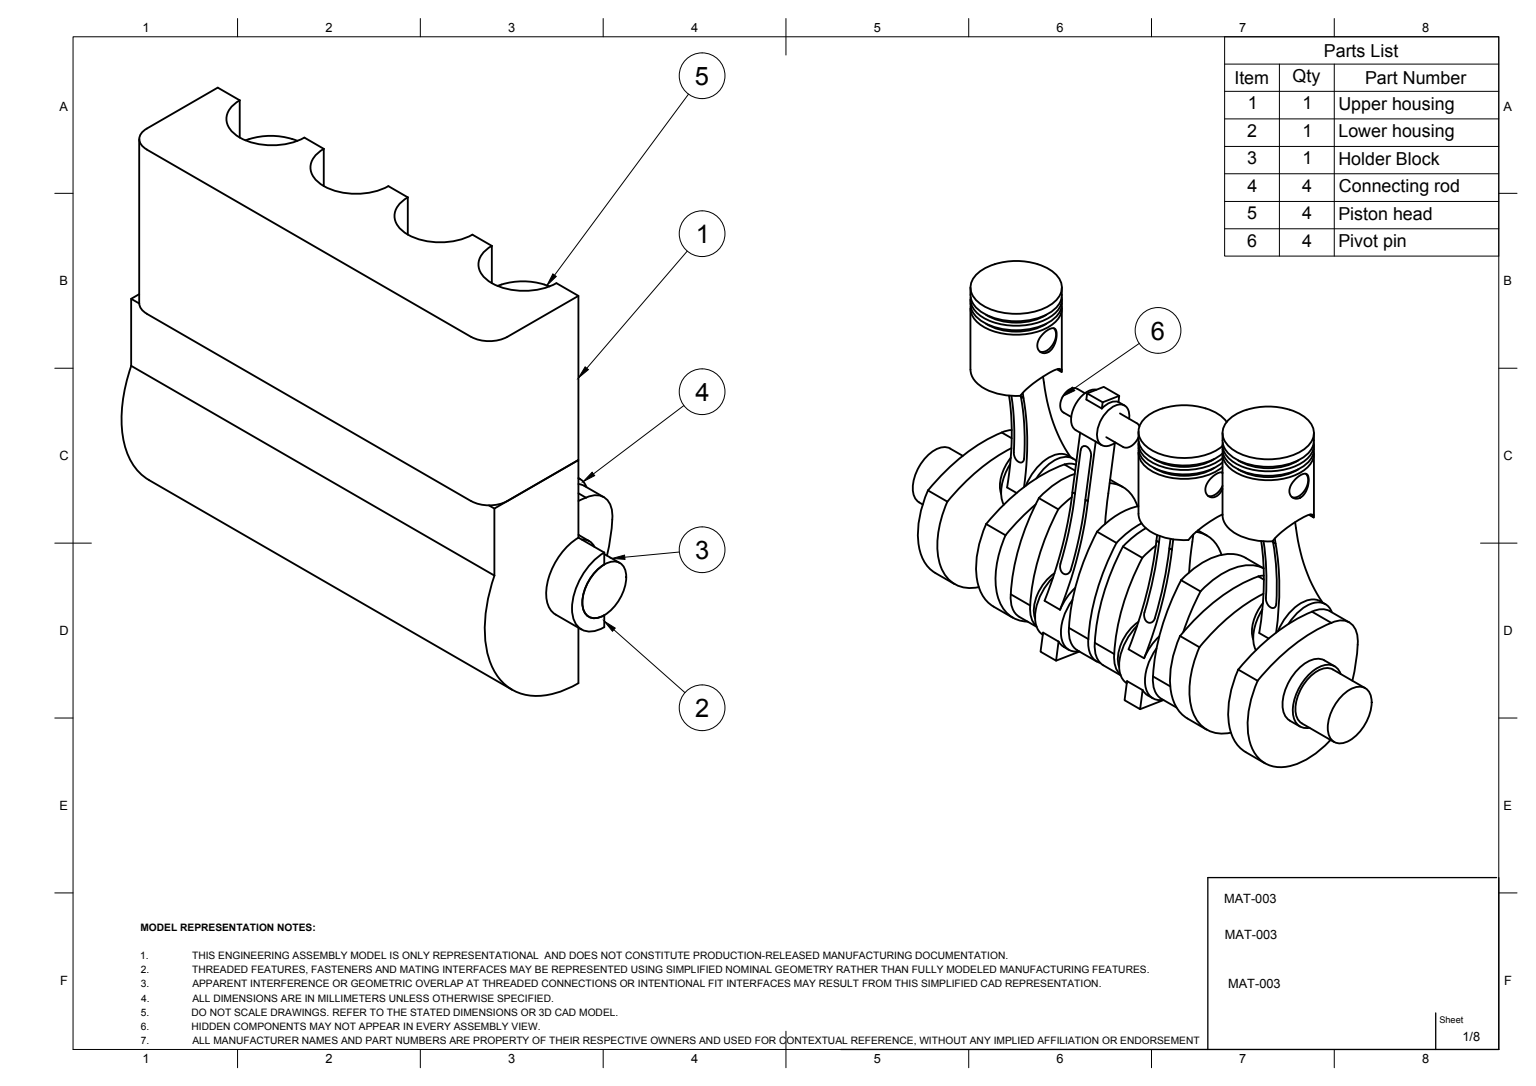
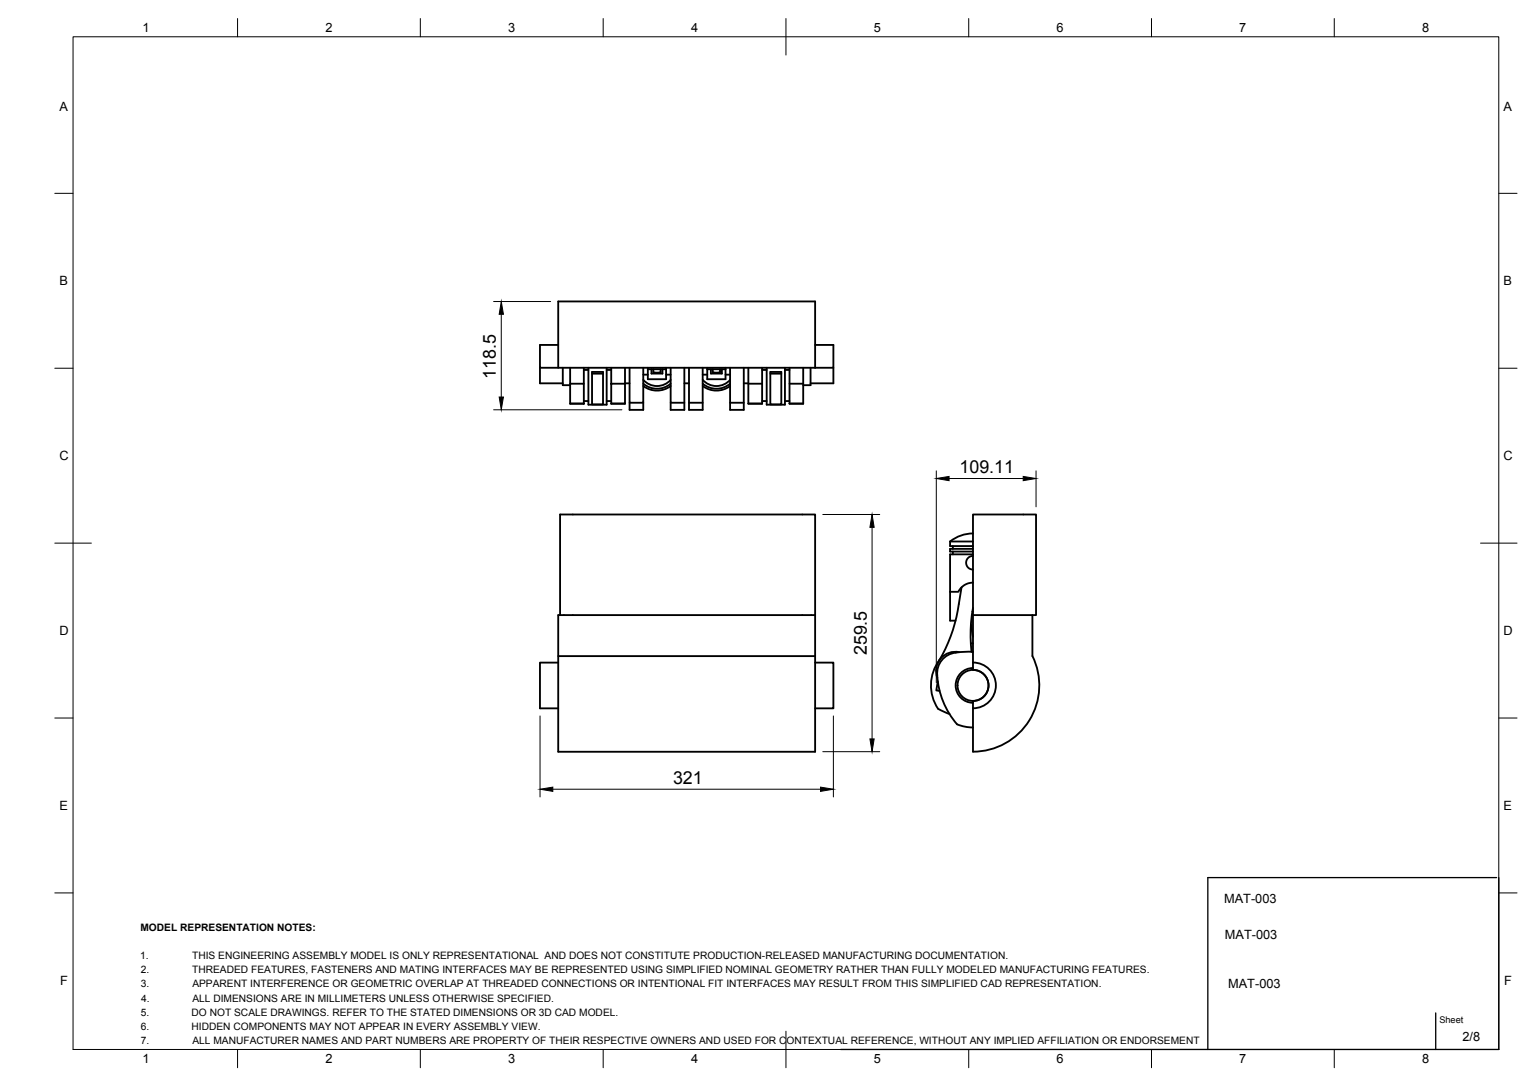
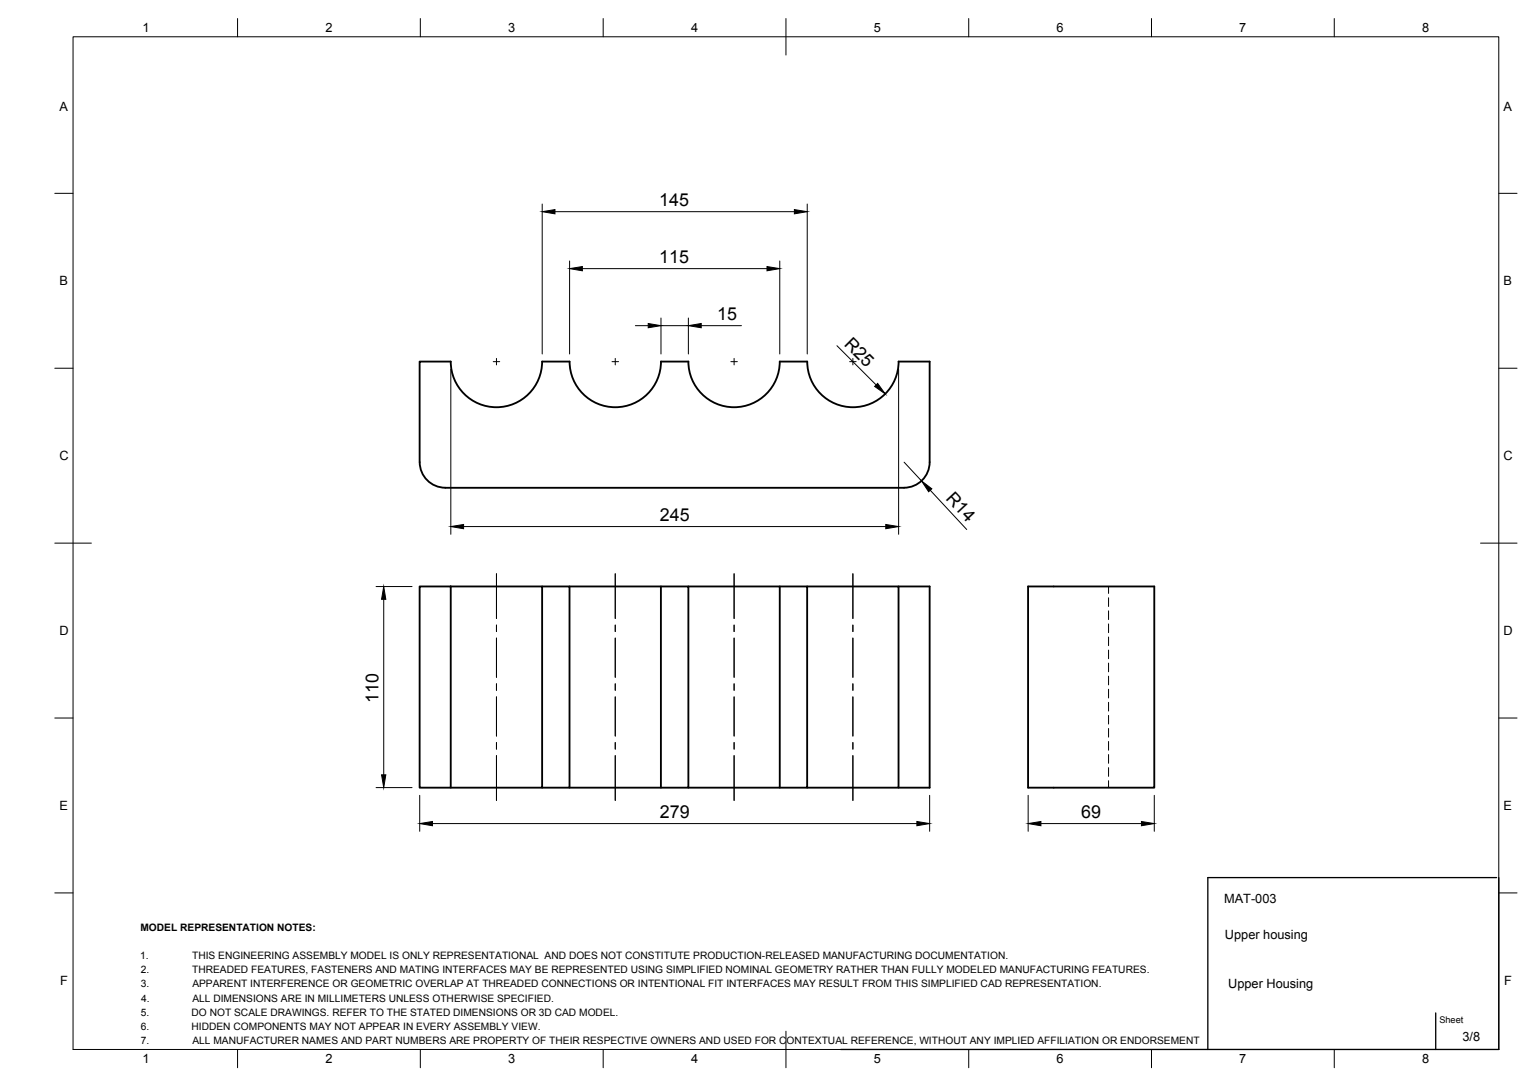
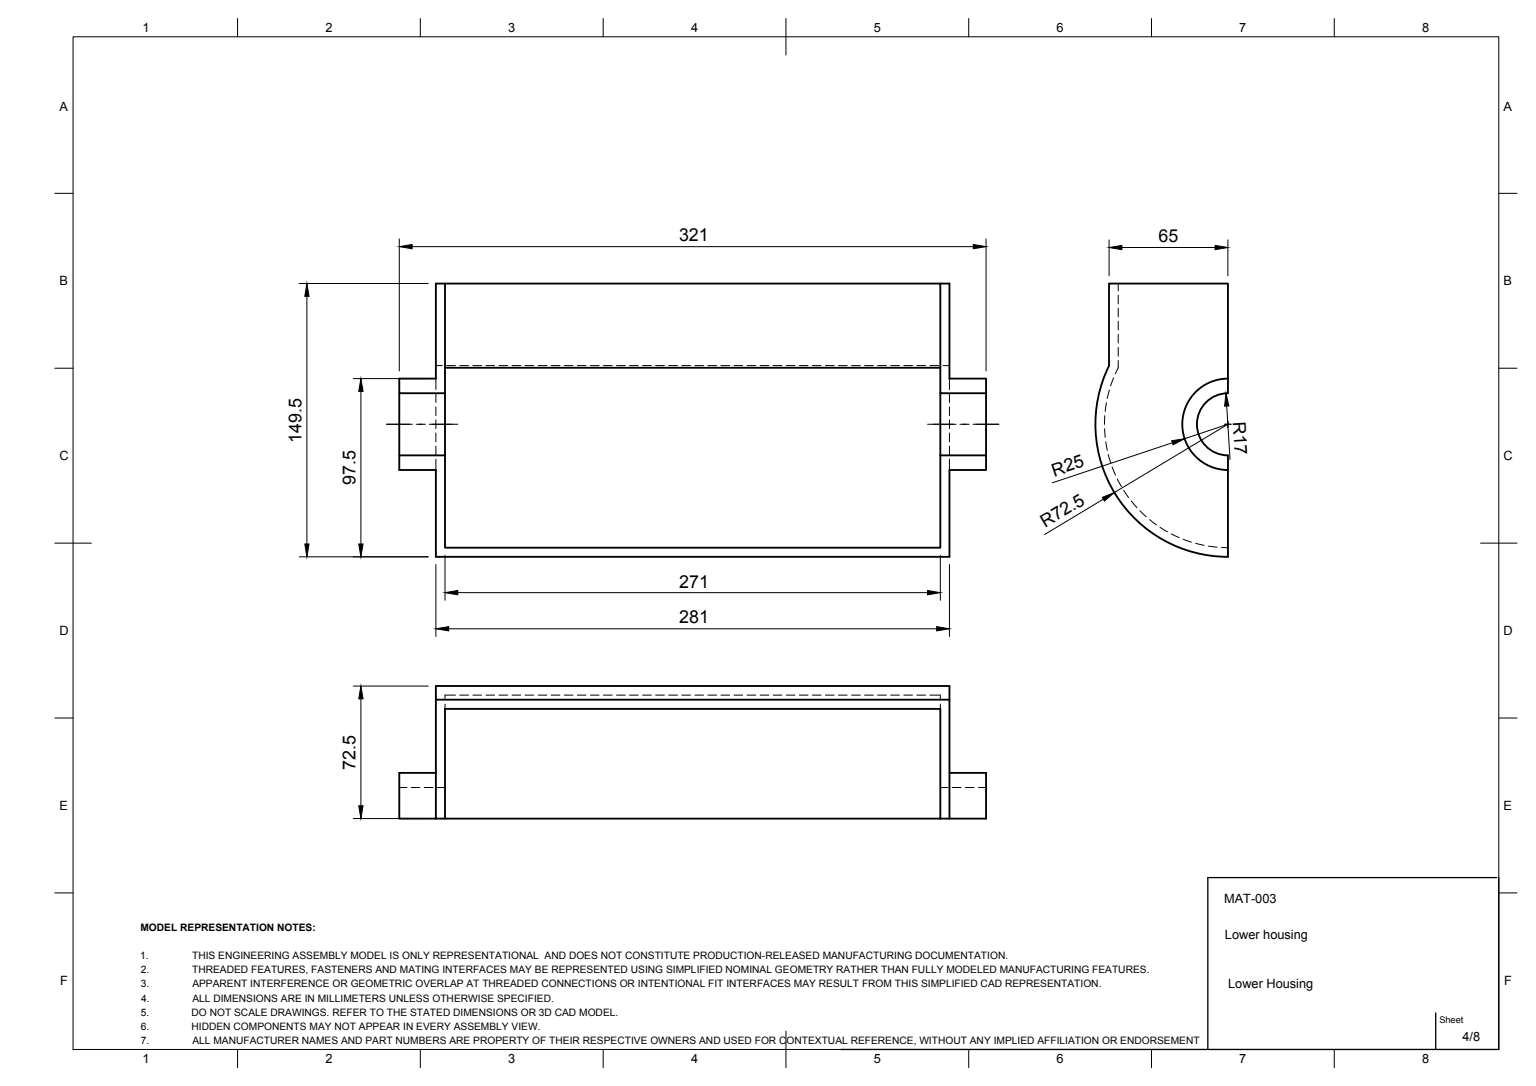
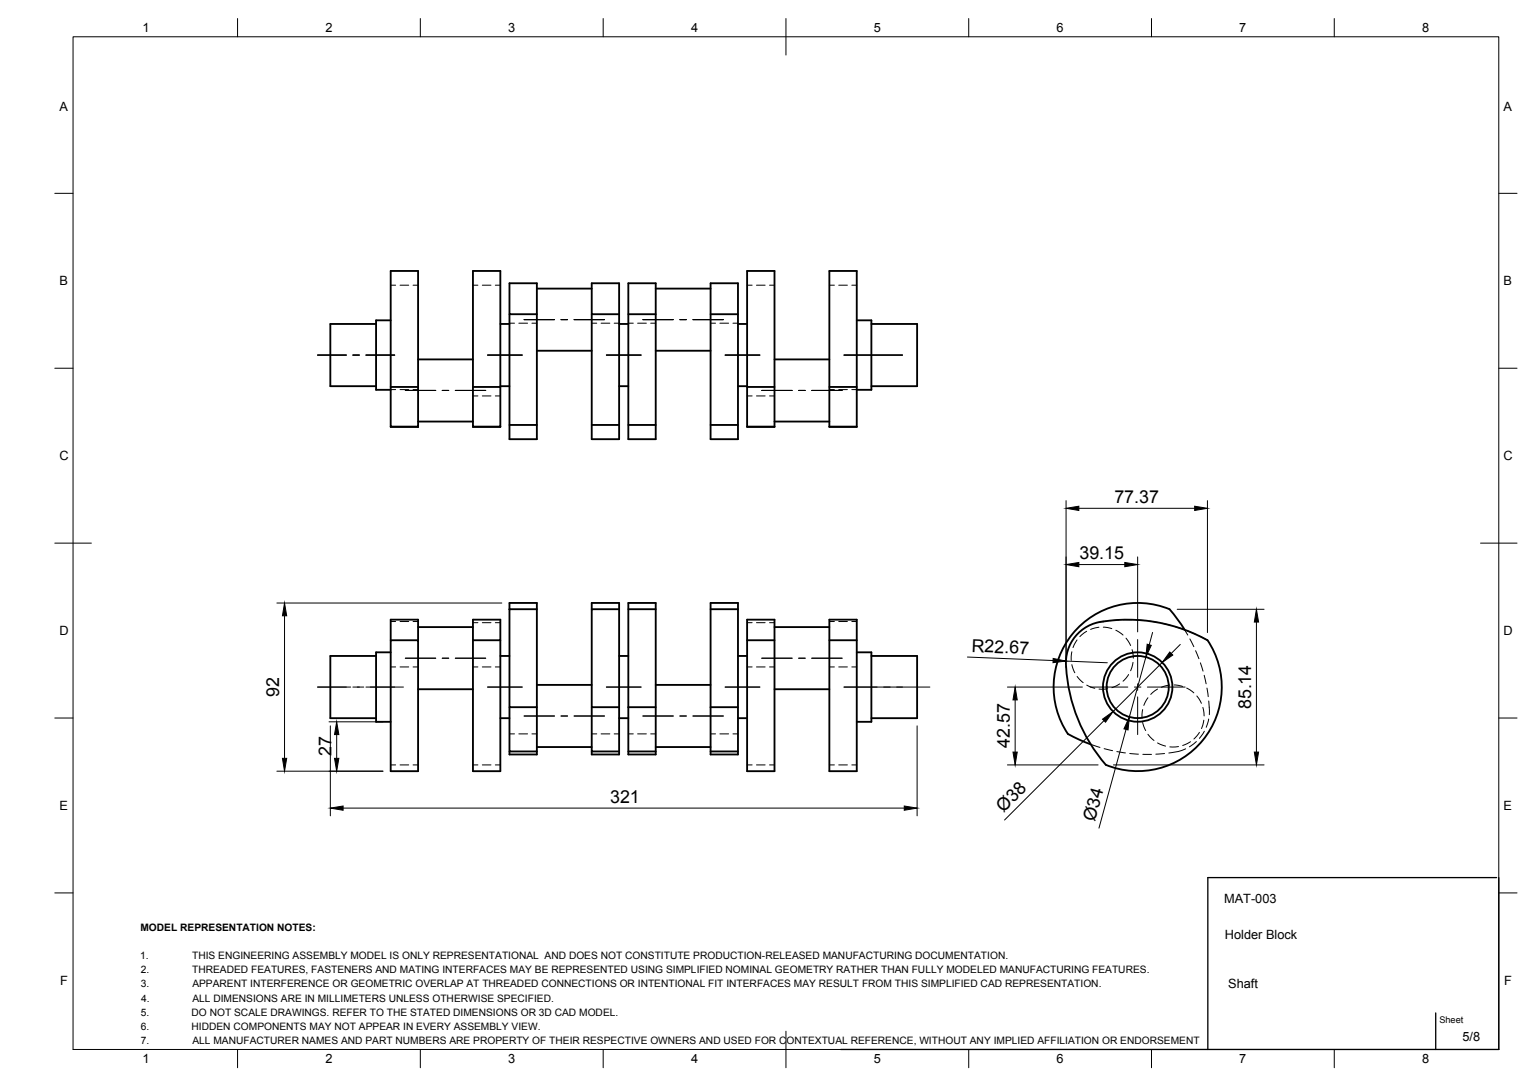
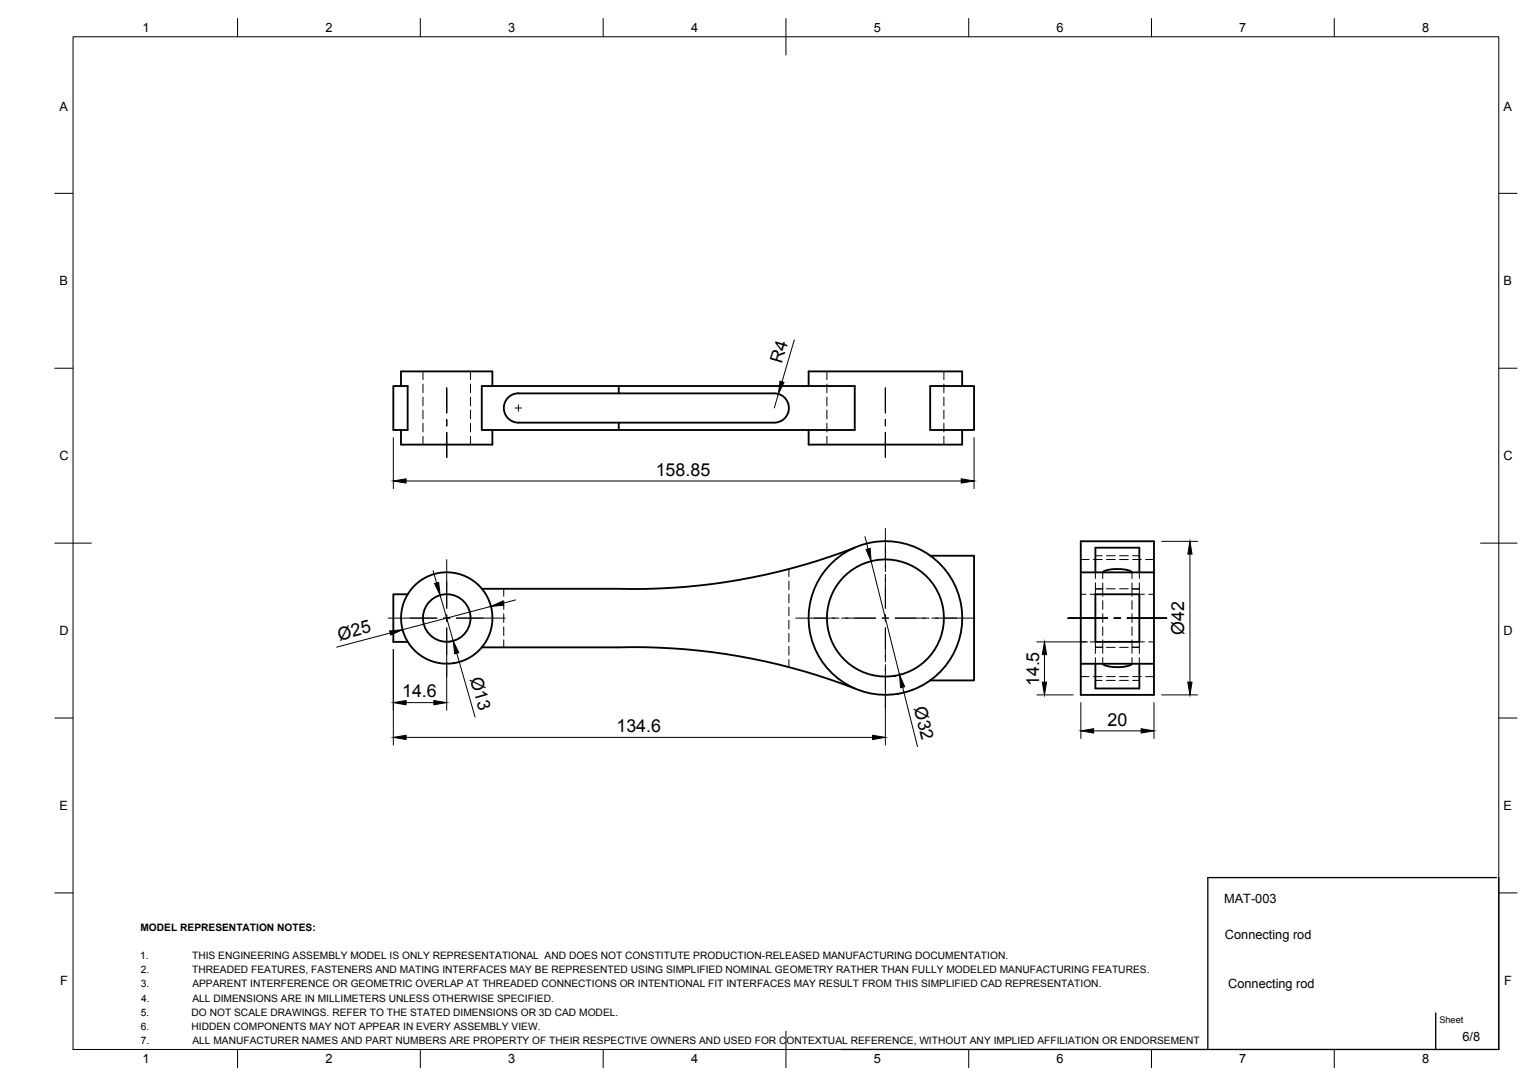
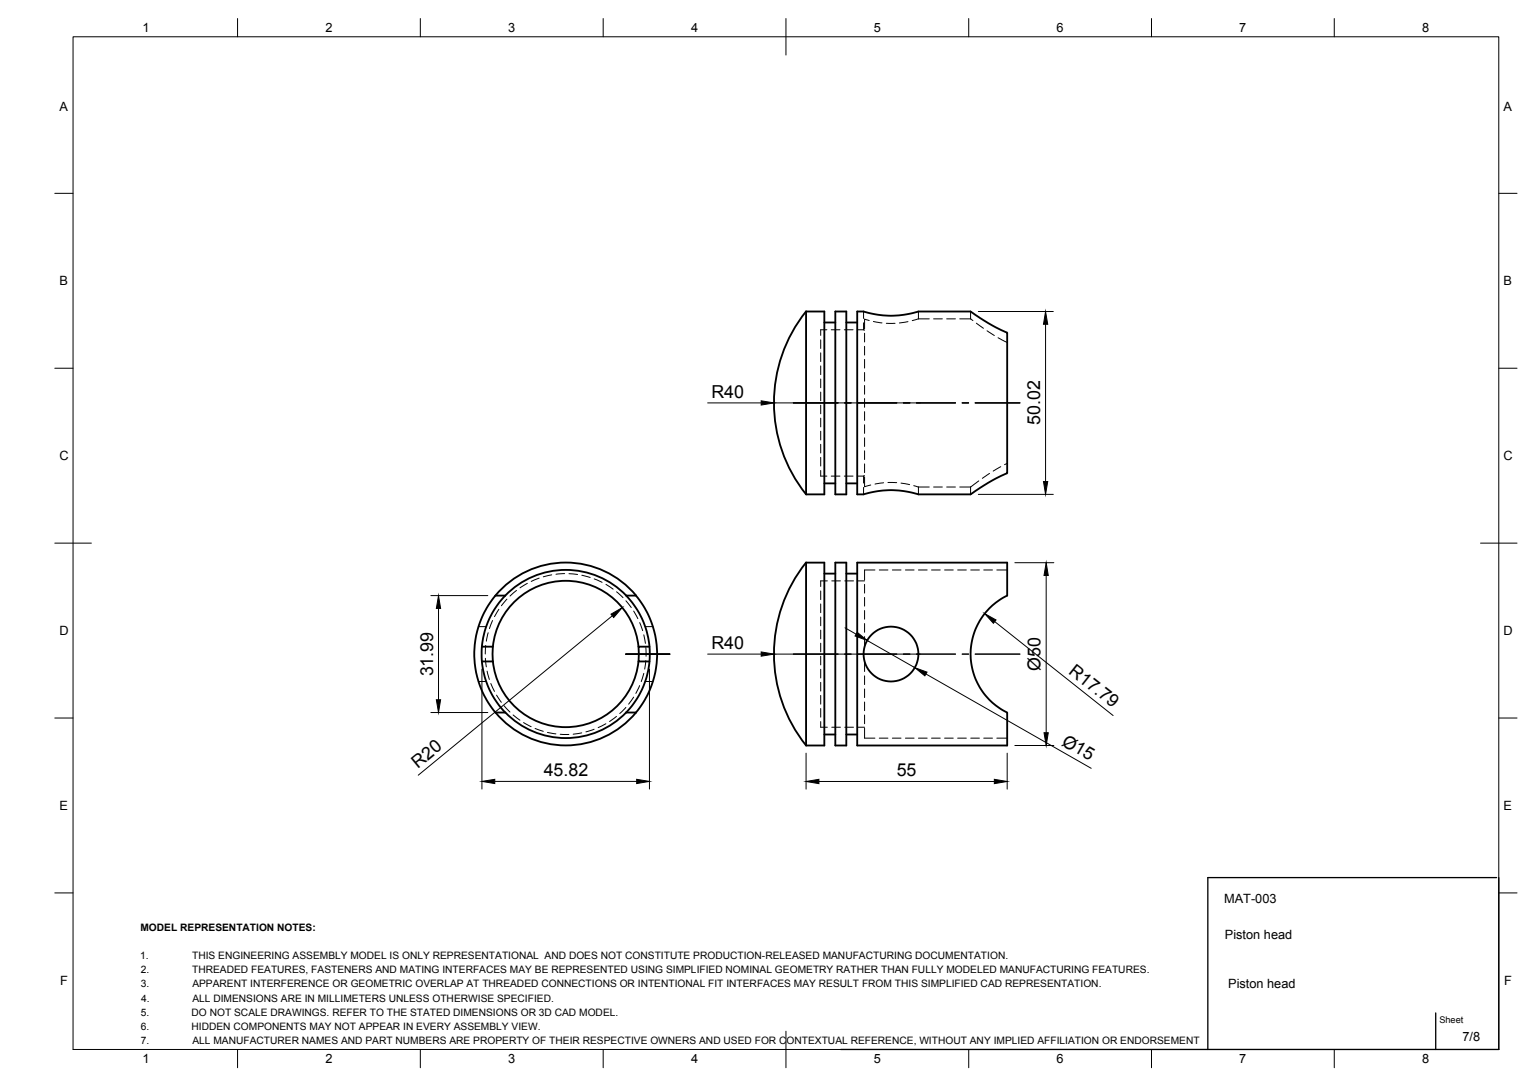
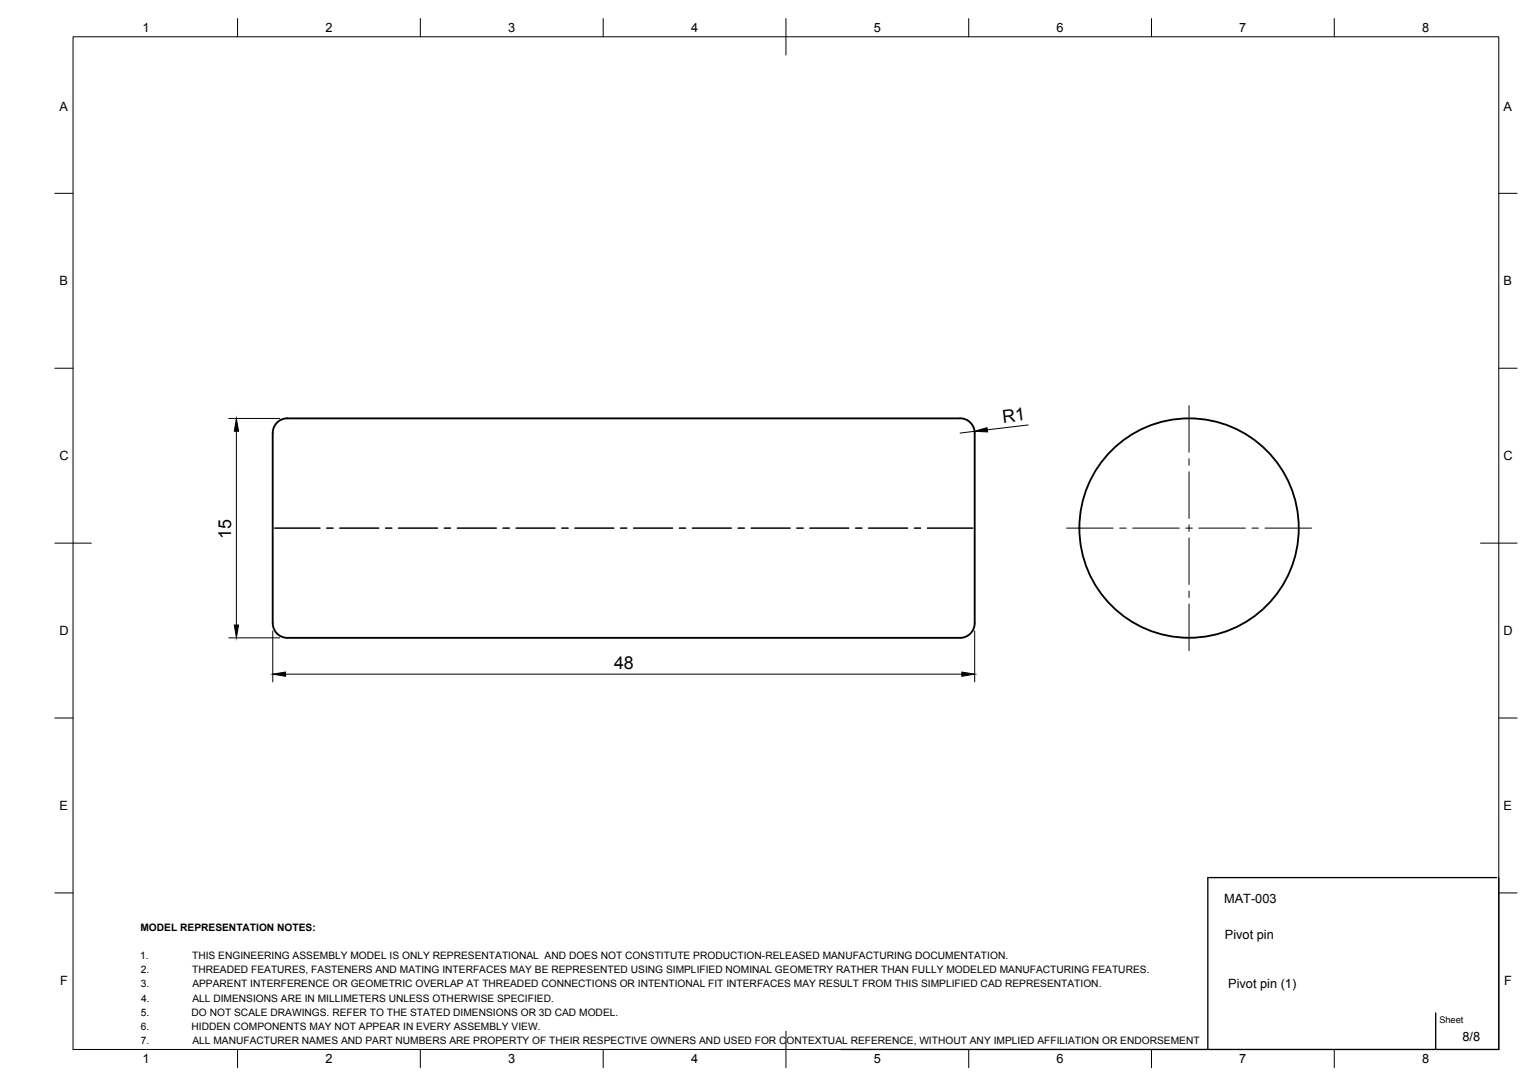
ISO-10303-21;
HEADER;
FILE_DESCRIPTION (('STEP AP214'),
    '1' );
FILE_NAME ('MAT-003',
    '2026-10-10T17:45:43',
    ( '' ),
    ( '' ),
    'SwSTEP 2.0',
    'SolidWorks 2024',
    '' );
FILE_SCHEMA (( 'AUTOMOTIVE_DESIGN' ));
ENDSEC;

DATA;
#1 = DIRECTION ( 'NONE',  ( -1.000000000000000000, 0.000000000000000000, 0.000000000000000000 ) ) ;
#2 = FACE_OUTER_BOUND ( 'NONE', #4262, .T. ) ;
#3 = FACE_OUTER_BOUND ( 'NONE', #4088, .T. ) ;
#4 = VERTEX_POINT ( 'NONE', #461 ) ;
#5 = DIRECTION ( 'NONE',  ( -0.000000000000000000, -0.000000000000000000, -1.000000000000000000 ) ) ;
#6 = AXIS2_PLACEMENT_3D ( 'NONE', #2010, #2938, #1015 ) ;
#7 = PLANE ( 'NONE',  #4575 ) ;
#8 = EDGE_CURVE ( 'NONE', #1209, #6017, #4433, .T. ) ;
#9 = VECTOR ( 'NONE', #5251, 1000.000000000000000 ) ;
#10 = CARTESIAN_POINT ( 'NONE',  ( -13.19762691892552731, 27.23125096863189754, 3.538843351020405148 ) ) ;
#11 = DIRECTION ( 'NONE',  ( -0.000000000000000000, 0.000000000000000000, 1.000000000000000000 ) ) ;
#12 = VERTEX_POINT ( 'NONE', #3966 ) ;
#13 = ORIENTED_EDGE ( 'NONE', *, *, #1970, .T. ) ;
#14 = FACE_OUTER_BOUND ( 'NONE', #2521, .T. ) ;
#15 = AXIS2_PLACEMENT_3D ( 'NONE', #2990, #2506, #3108 ) ;
#16 = FACE_OUTER_BOUND ( 'NONE', #1831, .T. ) ;
#17 = DIRECTION ( 'NONE',  ( -0.000000000000000000, -0.000000000000000000, -1.000000000000000000 ) ) ;
#18 = DIRECTION ( 'NONE',  ( 0.000000000000000000, 1.000000000000000000, 0.000000000000000000 ) ) ;
#19 = EDGE_LOOP ( 'NONE', ( #1698, #4393, #5502, #3759 ) ) ;
#20 = ORIENTED_EDGE ( 'NONE', *, *, #5697, .F. ) ;
#21 = ORIENTED_EDGE ( 'NONE', *, *, #6307, .T. ) ;
#22 = VECTOR ( 'NONE', #3280, 1000.000000000000000 ) ;
#23 = EDGE_CURVE ( 'NONE', #4236, #5003, #2060, .T. ) ;
#24 = DIRECTION ( 'NONE',  ( -0.000000000000000000, -0.000000000000000000, -1.000000000000000000 ) ) ;
#25 = FACE_OUTER_BOUND ( 'NONE', #4505, .T. ) ;
#26 = CARTESIAN_POINT ( 'NONE',  ( 12.21008954351328413, -21.81796696573389127, 5.154724438801038922 ) ) ;
#27 = ORIENTED_EDGE ( 'NONE', *, *, #299, .F. ) ;
#28 = EDGE_CURVE ( 'NONE', #3551, #1184, #4957, .T. ) ;
#29 = EDGE_CURVE ( 'NONE', #4703, #6200, #2516, .T. ) ;
#30 = DIRECTION ( 'NONE',  ( 1.083164259081603456E-16, -1.000000000000000000, 0.000000000000000000 ) ) ;
#31 = CARTESIAN_POINT ( 'NONE',  ( -6.979603745006294879, -21.91560538710199779, 29.02082494059217765 ) ) ;
#32 = EDGE_CURVE ( 'NONE', #4635, #4613, #1964, .T. ) ;
#33 = CARTESIAN_POINT ( 'NONE',  ( 20.00000000000000000, 2.449293598294706513E-15, 39.00000000000001421 ) ) ;
#34 = EDGE_LOOP ( 'NONE', ( #4986, #287, #6272, #1228, #2299, #5503, #2724 ) ) ;
#35 = CARTESIAN_POINT ( 'NONE',  ( 0.000000000000000000, 25.00000000000000000, -30.00000000000000000 ) ) ;
#36 = CIRCLE ( 'NONE', #3210, 17.00000000000000000 ) ;
#37 = CARTESIAN_POINT ( 'NONE',  ( 172.0000000000000000, 68.99999999999998579, 0.000000000000000000 ) ) ;
#38 = B_SPLINE_CURVE_WITH_KNOTS ( 'NONE', 3,
 ( #1697, #6029, #719, #3151, #3705, #4112 ),
 .UNSPECIFIED., .F., .F.,
 ( 4, 2, 4 ),
 ( 0.002032958594636734458, 0.003043324567219494060, 0.004053690539802253662 ),
 .UNSPECIFIED. ) ;
#39 = B_SPLINE_CURVE_WITH_KNOTS ( 'NONE', 3,
 ( #3746, #4279, #1287, #1358, #4178, #783, #2350, #6257, #5782, #1842, #3804, #4739, #3314, #2826, #6155, #5224, #4801, #3253, #3221, #2727, #816, #3709, #5194, #4704, #300, #337, #4247, #6228, #4964, #531, #2445, #3864, #5907, #2482, #4446, #3838, #2858, #3480, #4377, #429, #1973, #1033 ),
 .UNSPECIFIED., .F., .F.,
 ( 4, 2, 2, 2, 2, 2, 2, 2, 2, 2, 2, 2, 2, 2, 2, 2, 2, 2, 2, 2, 4 ),
 ( 0.02358501416070326803, 0.02505868070871360154, 0.02653234725672393851, 0.02800601380473427202, 0.02947968035274460899, 0.03021651362674978442, 0.03095334690075495637, 0.03242701344876530722, 0.03390067999677565114, 0.03463751327078083003, 0.03537434654478600199, 0.03684801309279635284, 0.03758484636680152480, 0.03832167964080669675, 0.03979534618881705454, 0.04126901273682739846, 0.04200584601083257735, 0.04274267928483775625, 0.04421634583284810710, 0.04569001238085845795, 0.04716367892886881574 ),
 .UNSPECIFIED. ) ;
#40 = EDGE_CURVE ( 'NONE', #2876, #1030, #4508, .T. ) ;
#41 = CARTESIAN_POINT ( 'NONE',  ( -16.23652742703189489, -37.28747423195188304, -115.0000000000000000 ) ) ;
#42 = LINE ( 'NONE', #1036, #6075 ) ;
#43 = VERTEX_POINT ( 'NONE', #1427 ) ;
#44 = CARTESIAN_POINT ( 'NONE',  ( 15.23842499831731523, 17.23716120365648052, 1.424676953056493112 ) ) ;
#45 = ORIENTED_EDGE ( 'NONE', *, *, #5504, .T. ) ;
#46 = CARTESIAN_POINT ( 'NONE',  ( -174.7835321302054865, 68.75545066608756883, 12.00000000000000000 ) ) ;
#47 = EDGE_CURVE ( 'NONE', #5003, #1574, #1946, .T. ) ;
#48 = CARTESIAN_POINT ( 'NONE',  ( 73.99999999999987210, 76.99999716619419132, 276.0000000000000000 ) ) ;
#49 = CARTESIAN_POINT ( 'NONE',  ( 17.00000000000000000, 25.00000000000000000, 0.000000000000000000 ) ) ;
#50 = CARTESIAN_POINT ( 'NONE',  ( 64.99991398172927859, 76.99999716619419132, 1.734723475976807094E-15 ) ) ;
#51 = VERTEX_POINT ( 'NONE', #3905 ) ;
#52 = EDGE_LOOP ( 'NONE', ( #3560, #240, #914, #1362 ) ) ;
#53 = VERTEX_POINT ( 'NONE', #142 ) ;
#54 = CARTESIAN_POINT ( 'NONE',  ( 15.99408614349810698, 25.00000000000000000, 0.000000000000000000 ) ) ;
#55 = CARTESIAN_POINT ( 'NONE',  ( -3.061616997868383043E-15, -25.00000000000000000, -65.00000000000000000 ) ) ;
#56 = CARTESIAN_POINT ( 'NONE',  ( -10.32035317195590984, -22.78260342671239869, 6.723738260341698414 ) ) ;
#57 = ORIENTED_EDGE ( 'NONE', *, *, #61, .F. ) ;
#58 = CARTESIAN_POINT ( 'NONE',  ( 31.31180517104795058, 82.87638965790611678, 249.6200851762758077 ) ) ;
#59 = CARTESIAN_POINT ( 'NONE',  ( -7.460990961498263019, -21.75625611239105694, 30.97809455494030928 ) ) ;
#60 = AXIS2_PLACEMENT_3D ( 'NONE', #399, #4931, #2444 ) ;
#61 = EDGE_CURVE ( 'NONE', #5090, #3913, #5607, .T. ) ;
#62 = LINE ( 'NONE', #3376, #3089 ) ;
#63 = ORIENTED_EDGE ( 'NONE', *, *, #4361, .F. ) ;
#64 = B_SPLINE_CURVE_WITH_KNOTS ( 'NONE', 3,
 ( #996, #2949, #3883, #2468, #3228, #4436, #1895, #26, #1990, #4334, #964, #3954, #5828, #5441, #1405, #4365, #5381, #2913, #1023, #549, #5470, #2986, #4820, #446, #5345, #3979, #3401, #2885, #1536, #6336, #4954, #5863, #2503, #4462, #1441, #56, #4887, #4402, #1076, #3622, #4555, #3530, #1685, #4981, #1140, #4096 ),
 .UNSPECIFIED., .F., .F.,
 ( 4, 2, 2, 2, 2, 2, 2, 2, 2, 2, 2, 2, 2, 2, 2, 2, 2, 2, 2, 2, 2, 2, 4 ),
 ( 9.772241184477329324E-19, 0.002589099528182565047, 0.005178199056365129227, 0.006472748820456409799, 0.007767298584547690371, 0.01035639811273024805, 0.01294549764091280919, 0.01424004740500408803, 0.01553459716909536686, 0.01812369669727792107, 0.01941824646136919991, 0.02071279622546047527, 0.02330189575364303295, 0.02459644551773431179, 0.02589099528182559062, 0.02848009481000814483, 0.02977464457409942367, 0.03106919433819069556, 0.03365829386637325671, 0.03495284363046453902, 0.03624739339455581438, 0.03883649292273837206, 0.04142559245092092279 ),
 .UNSPECIFIED. ) ;
#65 = DIRECTION ( 'NONE',  ( 1.000000000000000000, 0.000000000000000000, 0.000000000000000000 ) ) ;
#66 = CIRCLE ( 'NONE', #4486, 12.50000000000001421 ) ;
#67 = LINE ( 'NONE', #4867, #280 ) ;
#68 = COLOUR_RGB ( '',0.7921568627450980005, 0.8196078431372548767, 0.9333333333333333481 ) ;
#69 = EDGE_CURVE ( 'NONE', #1244, #5377, #5049, .T. ) ;
#70 = DIRECTION ( 'NONE',  ( 1.000000000000000000, 0.000000000000000000, 0.000000000000000000 ) ) ;
#71 = ORIENTED_EDGE ( 'NONE', *, *, #5909, .F. ) ;
#72 = VECTOR ( 'NONE', #6322, 1000.000000000000000 ) ;
#73 = FACE_OUTER_BOUND ( 'NONE', #4700, .T. ) ;
#74 = ORIENTED_EDGE ( 'NONE', *, *, #5032, .F. ) ;
#75 = CARTESIAN_POINT ( 'NONE',  ( -0.4497709217647500868, 23.00000000000000355, 24.27501000028010836 ) ) ;
#76 = ADVANCED_FACE ( 'NONE', ( #261, #2578 ), #1123, .T. ) ;
#77 = EDGE_CURVE ( 'NONE', #5794, #1266, #2476, .T. ) ;
#78 = DIRECTION ( 'NONE',  ( -0.000000000000000000, -0.000000000000000000, -1.000000000000000000 ) ) ;
#79 = CARTESIAN_POINT ( 'NONE',  ( 0.000000000000000000, 0.000000000000000000, -240.0000000000000000 ) ) ;
#80 = ORIENTED_EDGE ( 'NONE', *, *, #5837, .T. ) ;
#81 = VERTEX_POINT ( 'NONE', #1223 ) ;
#82 = ORIENTED_EDGE ( 'NONE', *, *, #1705, .T. ) ;
#83 = AXIS2_PLACEMENT_3D ( 'NONE', #303, #4222, #3223 ) ;
#84 = DIRECTION ( 'NONE',  ( 0.000000000000000000, -1.000000000000000000, 0.000000000000000000 ) ) ;
#85 = CARTESIAN_POINT ( 'NONE',  ( 0.000000000000000000, 14.00000000000000000, 0.000000000000000000 ) ) ;
#86 = AXIS2_PLACEMENT_3D ( 'NONE', #5507, #2633, #4633 ) ;
#87 = CARTESIAN_POINT ( 'NONE',  ( 0.000000000000000000, 0.000000000000000000, 48.00000000000000000 ) ) ;
#88 = ORIENTED_EDGE ( 'NONE', *, *, #6209, .F. ) ;
#89 = VECTOR ( 'NONE', #705, 1000.000000000000000 ) ;
#90 = CARTESIAN_POINT ( 'NONE',  ( 0.000000000000000000, -25.00000000000000000, 301.0000000000000568 ) ) ;
#91 = APPLICATION_PROTOCOL_DEFINITION ( 'draft international standard', 'automotive_design', 1998, #867 ) ;
#92 = CARTESIAN_POINT ( 'NONE',  ( -1.353316873173488588, -19.96515186930334096, 39.18355504947043499 ) ) ;
#93 = AXIS2_PLACEMENT_3D ( 'NONE', #1355, #6255, #2382 ) ;
#94 = DIRECTION ( 'NONE',  ( 1.000000000000000000, 0.000000000000000000, 0.000000000000000000 ) ) ;
#95 = EDGE_LOOP ( 'NONE', ( #3114, #6152 ) ) ;
#96 = ORIENTED_EDGE ( 'NONE', *, *, #579, .F. ) ;
#97 = AXIS2_PLACEMENT_3D ( 'NONE', #4292, #3267, #2839 ) ;
#98 = DIRECTION ( 'NONE',  ( -0.000000000000000000, -0.000000000000000000, -1.000000000000000000 ) ) ;
#99 = VECTOR ( 'NONE', #1167, 1000.000000000000000 ) ;
#100 = EDGE_CURVE ( 'NONE', #5003, #2855, #4024, .T. ) ;
#101 = DIRECTION ( 'NONE',  ( 1.000000000000000000, 0.000000000000000000, 0.000000000000000000 ) ) ;
#102 = VECTOR ( 'NONE', #3614, 1000.000000000000000 ) ;
#103 = ADVANCED_BREP_SHAPE_REPRESENTATION ( '', ( #4609, #6349 ), #1927 ) ;
#104 = EDGE_CURVE ( 'NONE', #4120, #4159, #4047, .T. ) ;
#105 = DIRECTION ( 'NONE',  ( 0.000000000000000000, 0.000000000000000000, 1.000000000000000000 ) ) ;
#106 = ORIENTED_EDGE ( 'NONE', *, *, #2540, .F. ) ;
#107 = PRESENTATION_STYLE_ASSIGNMENT (( #4506 ) ) ;
#108 = EDGE_CURVE ( 'NONE', #4284, #2336, #4223, .T. ) ;
#109 = CARTESIAN_POINT ( 'NONE',  ( 279.0000000000000000, 0.000000000000000000, 110.0000000000000000 ) ) ;
#110 = CARTESIAN_POINT ( 'NONE',  ( 0.2247101425308446754, 23.00000000000000355, 24.27501000028010480 ) ) ;
#111 = AXIS2_PLACEMENT_3D ( 'NONE', #2275, #6279, #3332 ) ;
#112 = CARTESIAN_POINT ( 'NONE',  ( 64.99991398172927859, 32.11307465182860454, 281.0000000000000000 ) ) ;
#113 = DIRECTION ( 'NONE',  ( 0.000000000000000000, 0.000000000000000000, -1.000000000000000000 ) ) ;
#114 = ADVANCED_FACE ( 'NONE', ( #2699 ), #6095, .F. ) ;
#115 = VECTOR ( 'NONE', #1796, 1000.000000000000000 ) ;
#116 = VERTEX_POINT ( 'NONE', #626 ) ;
#117 = VERTEX_POINT ( 'NONE', #4668 ) ;
#118 = EDGE_CURVE ( 'NONE', #2855, #4195, #121, .T. ) ;
#119 = EDGE_LOOP ( 'NONE', ( #1237, #139, #1625, #1192 ) ) ;
#120 = CARTESIAN_POINT ( 'NONE',  ( 44.56092774862622719, -29.44644455561813956, -225.0000000000000000 ) ) ;
#121 = CIRCLE ( 'NONE', #637, 24.99999999999999289 ) ;
#122 = AXIS2_PLACEMENT_3D ( 'NONE', #5343, #2370, #5378 ) ;
#123 = CARTESIAN_POINT ( 'NONE',  ( 2.012341796004660122, 22.91179784512888773, 39.00000000000001421 ) ) ;
#124 = CARTESIAN_POINT ( 'NONE',  ( 44.56092774862622719, -29.44644455561813956, -240.0000000000000000 ) ) ;
#125 = EDGE_CURVE ( 'NONE', #1691, #43, #4114, .T. ) ;
#126 = CARTESIAN_POINT ( 'NONE',  ( 0.2052511266213299934, 21.25619793154162807, -45.00000000000000000 ) ) ;
#127 = DIRECTION ( 'NONE',  ( -0.000000000000000000, -0.000000000000000000, 1.000000000000000000 ) ) ;
#128 = ORIENTED_EDGE ( 'NONE', *, *, #3806, .T. ) ;
#129 = AXIS2_PLACEMENT_3D ( 'NONE', #4697, #291, #748 ) ;
#130 = EDGE_CURVE ( 'NONE', #2876, #3788, #5065, .T. ) ;
#131 = DIRECTION ( 'NONE',  ( -0.9999999999999998890, 1.376214178094281264E-17, 4.170629591220277657E-16 ) ) ;
#132 = DIRECTION ( 'NONE',  ( 0.000000000000000000, 1.000000000000000000, 1.247733429937938623E-16 ) ) ;
#133 = CARTESIAN_POINT ( 'NONE',  ( 0.000000000000000000, 0.000000000000000000, 0.000000000000000000 ) ) ;
#134 = ORIENTED_EDGE ( 'NONE', *, *, #595, .T. ) ;
#135 = LINE ( 'NONE', #1113, #2828 ) ;
#136 = UNCERTAINTY_MEASURE_WITH_UNIT (LENGTH_MEASURE( 1.000000000000000082E-05 ), #2437, 'distance_accuracy_value', 'NONE');
#137 = DIRECTION ( 'NONE',  ( -0.000000000000000000, 0.000000000000000000, 1.000000000000000000 ) ) ;
#138 = CYLINDRICAL_SURFACE ( 'NONE', #419, 23.00000000000000000 ) ;
#139 = ORIENTED_EDGE ( 'NONE', *, *, #2354, .F. ) ;
#140 = CARTESIAN_POINT ( 'NONE',  ( 59.99991398172927859, 0.000000000000000000, 281.0000000000000000 ) ) ;
#141 = CIRCLE ( 'NONE', #963, 25.00000000000000000 ) ;
#142 = CARTESIAN_POINT ( 'NONE',  ( -25.00000000000000000, 0.000000000000000000, 0.000000000000000000 ) ) ;
#143 = CARTESIAN_POINT ( 'NONE',  ( -7.491878387983184062, 21.74571065617575982, 31.20484628725278498 ) ) ;
#144 = CARTESIAN_POINT ( 'NONE',  ( 1.698285149303728536, 24.95717370495093945, 9.939986931234113143 ) ) ;
#145 = DIRECTION ( 'NONE',  ( 0.000000000000000000, -1.000000000000000000, 0.000000000000000000 ) ) ;
#146 = VERTEX_POINT ( 'NONE', #1090 ) ;
#147 = ORIENTED_EDGE ( 'NONE', *, *, #6162, .F. ) ;
#148 = ORIENTED_EDGE ( 'NONE', *, *, #974, .F. ) ;
#149 = LINE ( 'NONE', #216, #2805 ) ;
#150 = B_SPLINE_CURVE_WITH_KNOTS ( 'NONE', 3,
 ( #3485, #592, #44, #5457, #3004, #2543, #6001, #2576, #4969, #1575, #4536, #5913, #2094, #979, #2927, #4904, #500, #2450, #1978, #2215, #721, #6123, #4046, #6065, #6032, #5579, #1121, #5643, #2608, #6153, #5126, #1608, #754, #297, #3573, #3219, #1740, #5192, #1644, #234, #5544, #4175 ),
 .UNSPECIFIED., .F., .F.,
 ( 4, 2, 2, 2, 2, 2, 2, 2, 2, 2, 2, 2, 2, 2, 2, 2, 2, 2, 2, 2, 4 ),
 ( 0.000000000000000000, 0.002617858692138167777, 0.005235717384276335554, 0.006544646730345418141, 0.007853576076414500728, 0.01047143476855266243, 0.01308929346069082240, 0.01439822280675990239, 0.01570715215282898758, 0.01832501084496714408, 0.01963394019103622407, 0.02094286953710530058, 0.02356072822924346055, 0.02486965757531254054, 0.02617858692138162399, 0.02879644561351977702, 0.03141430430565794046, 0.03403216299779609350, 0.03665002168993425347, 0.03926788038207241344, 0.04188573907421057341 ),
 .UNSPECIFIED. ) ;
#151 = MANIFOLD_SOLID_BREP ( 'Cut-Extrude1', #5264 ) ;
#152 = CARTESIAN_POINT ( 'NONE',  ( -6.500000000000000000, 134.5953136438507158, 12.00000000000000000 ) ) ;
#153 = DIRECTION ( 'NONE',  ( -0.000000000000000000, -0.000000000000000000, -1.000000000000000000 ) ) ;
#154 = DIRECTION ( 'NONE',  ( -1.000000000000000000, 0.000000000000000000, 0.000000000000000000 ) ) ;
#155 =( GEOMETRIC_REPRESENTATION_CONTEXT ( 3 ) GLOBAL_UNCERTAINTY_ASSIGNED_CONTEXT ( ( #1737 ) ) GLOBAL_UNIT_ASSIGNED_CONTEXT ( ( #6051, #2054, #4037 ) ) REPRESENTATION_CONTEXT ( 'NONE', 'WORKASPACE' ) );
#156 = CYLINDRICAL_SURFACE ( 'NONE', #3481, 4.000000000000000000 ) ;
#157 = VERTEX_POINT ( 'NONE', #5580 ) ;
#158 = FACE_OUTER_BOUND ( 'NONE', #3418, .T. ) ;
#159 = PRODUCT_CONTEXT ( 'NONE', #5893, 'mechanical' ) ;
#160 = LINE ( 'NONE', #6020, #2209 ) ;
#161 = VERTEX_POINT ( 'NONE', #2156 ) ;
#162 = CARTESIAN_POINT ( 'NONE',  ( 0.000000000000000000, 0.000000000000000000, 51.00000000000002842 ) ) ;
#163 = ORIENTED_EDGE ( 'NONE', *, *, #395, .F. ) ;
#164 = DIRECTION ( 'NONE',  ( -0.000000000000000000, -0.000000000000000000, 1.000000000000000000 ) ) ;
#165 = FACE_OUTER_BOUND ( 'NONE', #2771, .T. ) ;
#166 = AXIS2_PLACEMENT_3D ( 'NONE', #680, #1059, #2631 ) ;
#167 = APPLICATION_CONTEXT ( 'automotive_design' ) ;
#168 = DIRECTION ( 'NONE',  ( 1.000000000000000000, 0.000000000000000000, 0.000000000000000000 ) ) ;
#169 = CIRCLE ( 'NONE', #5615, 166.8359700257217071 ) ;
#170 = FACE_OUTER_BOUND ( 'NONE', #5424, .T. ) ;
#171 = ORIENTED_EDGE ( 'NONE', *, *, #4573, .F. ) ;
#172 = CARTESIAN_POINT ( 'NONE',  ( 67.00000000000000000, 69.00000000000000000, 110.0000000000000000 ) ) ;
#173 =( NAMED_UNIT ( * ) PLANE_ANGLE_UNIT ( ) SI_UNIT ( $, .RADIAN. ) );
#174 = CARTESIAN_POINT ( 'NONE',  ( -7.269041597172756219, 21.82161019007790514, 29.87399971471650062 ) ) ;
#175 = AXIS2_PLACEMENT_3D ( 'NONE', #388, #2953, #1897 ) ;
#176 = CARTESIAN_POINT ( 'NONE',  ( -5.944036167333009324, 24.28654258472968763, 8.982995935198127668 ) ) ;
#177 = DIRECTION ( 'NONE',  ( -0.000000000000000000, -0.000000000000000000, -1.000000000000000000 ) ) ;
#178 = EDGE_LOOP ( 'NONE', ( #2214, #4560 ) ) ;
#179 = EDGE_LOOP ( 'NONE', ( #3932, #3010 ) ) ;
#180 = CARTESIAN_POINT ( 'NONE',  ( -17.00000000000000000, 2.081899558550500280E-15, -273.0000000000000000 ) ) ;
#181 = DIRECTION ( 'NONE',  ( -0.000000000000000000, -0.000000000000000000, -1.000000000000000000 ) ) ;
#182 = DIRECTION ( 'NONE',  ( 0.000000000000000000, 1.000000000000000000, -1.284980352575412668E-17 ) ) ;
#183 = DIRECTION ( 'NONE',  ( -0.000000000000000000, -0.000000000000000000, 1.000000000000000000 ) ) ;
#184 = AXIS2_PLACEMENT_3D ( 'NONE', #1992, #4465, #2529 ) ;
#185 = PLANE ( 'NONE',  #3886 ) ;
#186 = ORIENTED_EDGE ( 'NONE', *, *, #4679, .F. ) ;
#187 = EDGE_CURVE ( 'NONE', #1008, #2831, #3637, .T. ) ;
#188 = AXIS2_PLACEMENT_3D ( 'NONE', #6357, #4909, #956 ) ;
#189 = EDGE_CURVE ( 'NONE', #3628, #146, #1775, .T. ) ;
#190 = CARTESIAN_POINT ( 'NONE',  ( -2.450084894395748503, -22.87335089571185875, 38.87807751528530531 ) ) ;
#191 = EDGE_CURVE ( 'NONE', #3657, #5057, #2480, .T. ) ;
#192 = EDGE_LOOP ( 'NONE', ( #4807, #5234, #4644, #6295 ) ) ;
#193 = FACE_OUTER_BOUND ( 'NONE', #676, .T. ) ;
#194 = ORIENTED_EDGE ( 'NONE', *, *, #3413, .T. ) ;
#195 = CIRCLE ( 'NONE', #5537, 17.00000000000000000 ) ;
#196 = EDGE_CURVE ( 'NONE', #1460, #3708, #4019, .T. ) ;
#197 = ADVANCED_FACE ( 'NONE', ( #3287 ), #5676, .F. ) ;
#198 = CARTESIAN_POINT ( 'NONE',  ( 0.000000000000000000, 14.00000000000000000, 110.0000000000000000 ) ) ;
#199 = CARTESIAN_POINT ( 'NONE',  ( -22.21770253897231839, -3.871672004621880436, 0.000000000000000000 ) ) ;
#200 = AXIS2_PLACEMENT_3D ( 'NONE', #653, #2670, #3094 ) ;
#201 = DIRECTION ( 'NONE',  ( 1.000000000000000000, 0.000000000000000000, 0.000000000000000000 ) ) ;
#202 = CARTESIAN_POINT ( 'NONE',  ( 0.000000000000000000, 0.000000000000000000, 0.000000000000000000 ) ) ;
#203 = EDGE_LOOP ( 'NONE', ( #3143, #5565 ) ) ;
#204 = LINE ( 'NONE', #2155, #1735 ) ;
#205 = CIRCLE ( 'NONE', #3492, 45.99999999999997868 ) ;
#206 = DIRECTION ( 'NONE',  ( -0.000000000000000000, -0.000000000000000000, 1.000000000000000000 ) ) ;
#207 = CARTESIAN_POINT ( 'NONE',  ( -3.466163672723409750, 22.74070890941651157, 25.10873389944362444 ) ) ;
#208 = ADVANCED_FACE ( 'NONE', ( #366 ), #2251, .F. ) ;
#209 = CIRCLE ( 'NONE', #6273, 23.00000000000000000 ) ;
#210 = CARTESIAN_POINT ( 'NONE',  ( -13.06023069425439509, 21.31967003585100784, 4.296371343529790110 ) ) ;
#211 = CARTESIAN_POINT ( 'NONE',  ( 3.471216600621237713, -22.73745234227088829, 38.42710443719838054 ) ) ;
#212 = ORIENTED_EDGE ( 'NONE', *, *, #4955, .F. ) ;
#213 = ORIENTED_EDGE ( 'NONE', *, *, #6031, .T. ) ;
#214 = VERTEX_POINT ( 'NONE', #1745 ) ;
#215 = AXIS2_PLACEMENT_3D ( 'NONE', #4568, #5162, #623 ) ;
#216 = CARTESIAN_POINT ( 'NONE',  ( 0.000000000000000000, 76.99999716619419132, 5.000000000000000000 ) ) ;
#217 = CARTESIAN_POINT ( 'NONE',  ( 44.00000000000008527, 13.41640786499836224, -160.0000000000000284 ) ) ;
#218 = DIRECTION ( 'NONE',  ( -0.000000000000000000, -0.000000000000000000, -1.000000000000000000 ) ) ;
#219 = CYLINDRICAL_SURFACE ( 'NONE', #1741, 17.79053956122086078 ) ;
#220 = CARTESIAN_POINT ( 'NONE',  ( 44.43364355155687662, -29.42304313293534790, -45.00000000000000000 ) ) ;
#221 = VERTEX_POINT ( 'NONE', #5746 ) ;
#222 = EDGE_CURVE ( 'NONE', #2940, #959, #39, .T. ) ;
#223 = CARTESIAN_POINT ( 'NONE',  ( -15.63711455316257215, -16.87386736187478675, 0.7328676451471519693 ) ) ;
#224 = ORIENTED_EDGE ( 'NONE', *, *, #2464, .T. ) ;
#225 = DIRECTION ( 'NONE',  ( -0.000000000000000000, 0.000000000000000000, 1.000000000000000000 ) ) ;
#226 = ORIENTED_EDGE ( 'NONE', *, *, #6094, .T. ) ;
#227 = VECTOR ( 'NONE', #4271, 1000.000000000000000 ) ;
#228 = SHAPE_REPRESENTATION_RELATIONSHIP ( 'NONE' , 'NONE' ,  #2313, #2933 ) ;
#229 = CARTESIAN_POINT ( 'NONE',  ( -0.2052511266214760433, -21.25619793154163517, -65.00000000000000000 ) ) ;
#230 = EDGE_CURVE ( 'NONE', #5659, #862, #5842, .T. ) ;
#231 = FACE_OUTER_BOUND ( 'NONE', #5250, .T. ) ;
#232 = CARTESIAN_POINT ( 'NONE',  ( 44.00000000000000000, -13.41640786499873705, -45.00000000000000000 ) ) ;
#233 = ORIENTED_EDGE ( 'NONE', *, *, #2398, .F. ) ;
#234 = CARTESIAN_POINT ( 'NONE',  ( -15.23263781889692048, 17.24245498722747527, 1.434805278142651463 ) ) ;
#235 = DIRECTION ( 'NONE',  ( -0.000000000000000000, -1.740526192617802767E-17, 1.000000000000000000 ) ) ;
#236 = DIRECTION ( 'NONE',  ( -0.000000000000000000, 0.000000000000000000, -1.000000000000000000 ) ) ;
#237 = DIRECTION ( 'NONE',  ( -1.000000000000000000, 0.000000000000000000, 0.000000000000000000 ) ) ;
#238 = DIRECTION ( 'NONE',  ( -1.000000000000000000, 0.000000000000000000, 0.000000000000000000 ) ) ;
#239 = ORIENTED_EDGE ( 'NONE', *, *, #5930, .F. ) ;
#240 = ORIENTED_EDGE ( 'NONE', *, *, #3676, .T. ) ;
#241 = CARTESIAN_POINT ( 'NONE',  ( 0.000000000000000000, 76.99999716619419132, 5.000000000000000000 ) ) ;
#242 = CARTESIAN_POINT ( 'NONE',  ( -0.2052511266214760433, -21.25619793154163517, -160.0000000000000284 ) ) ;
#243 = CARTESIAN_POINT ( 'NONE',  ( 0.000000000000000000, 0.000000000000000000, 55.00000000000000711 ) ) ;
#244 = DIRECTION ( 'NONE',  ( 0.000000000000000000, 0.000000000000000000, -1.000000000000000000 ) ) ;
#245 = FACE_OUTER_BOUND ( 'NONE', #526, .T. ) ;
#246 = EDGE_LOOP ( 'NONE', ( #2762, #958, #1397, #4692, #5981, #2970 ) ) ;
#247 = LINE ( 'NONE', #5691, #4727 ) ;
#248 = DIRECTION ( 'NONE',  ( 1.000000000000000000, 0.000000000000000000, 0.000000000000000000 ) ) ;
#249 = EDGE_CURVE ( 'NONE', #5856, #1997, #4067, .T. ) ;
#250 = ORIENTED_EDGE ( 'NONE', *, *, #4382, .T. ) ;
#251 = PRODUCT_DEFINITION_SHAPE ( 'NONE', 'NONE',  #6365 ) ;
#252 = DIRECTION ( 'NONE',  ( 1.000000000000000000, 0.000000000000000000, 0.000000000000000000 ) ) ;
#253 = ORIENTED_EDGE ( 'NONE', *, *, #3958, .T. ) ;
#254 = DIRECTION ( 'NONE',  ( 1.000000000000000000, 0.000000000000000000, 0.000000000000000000 ) ) ;
#255 = ADVANCED_FACE ( 'NONE', ( #6347, #3897 ), #5362, .T. ) ;
#256 = DIRECTION ( 'NONE',  ( 0.000000000000000000, 0.000000000000000000, 1.000000000000000000 ) ) ;
#257 = CARTESIAN_POINT ( 'NONE',  ( 174.7835321302054865, 68.75545066608756883, 12.00000000000000000 ) ) ;
#258 = VERTEX_POINT ( 'NONE', #1877 ) ;
#259 = DIRECTION ( 'NONE',  ( 0.000000000000000000, 0.000000000000000000, 1.000000000000000000 ) ) ;
#260 = EDGE_LOOP ( 'NONE', ( #5116, #2752, #3718, #1984 ) ) ;
#261 = FACE_OUTER_BOUND ( 'NONE', #2435, .T. ) ;
#262 = CARTESIAN_POINT ( 'NONE',  ( -44.00000000000000000, -13.41640786499873350, -180.0000000000000000 ) ) ;
#263 = AXIS2_PLACEMENT_3D ( 'NONE', #2565, #4526, #132 ) ;
#264 = EDGE_CURVE ( 'NONE', #775, #6000, #3921, .T. ) ;
#265 = CARTESIAN_POINT ( 'NONE',  ( 10.97130857767020551, 22.47473234318869828, 6.237739505811246588 ) ) ;
#267 = ADVANCED_FACE ( 'NONE', ( #945 ), #494, .T. ) ;
#266 = CARTESIAN_POINT ( 'NONE',  ( 5.116921499885075164, -22.42580359959007552, 37.27629952662707069 ) ) ;
#268 = ORIENTED_EDGE ( 'NONE', *, *, #3411, .F. ) ;
#269 = ORIENTED_EDGE ( 'NONE', *, *, #3444, .T. ) ;
#270 = CARTESIAN_POINT ( 'NONE',  ( -0.4986381067920973575, 25.00000000000001066, 24.27501000028010836 ) ) ;
#271 = ADVANCED_FACE ( 'NONE', ( #158 ), #1142, .T. ) ;
#272 = EDGE_CURVE ( 'NONE', #4432, #2238, #5083, .T. ) ;
#273 = LINE ( 'NONE', #4092, #6243 ) ;
#274 = CARTESIAN_POINT ( 'NONE',  ( 0.000000000000000000, 0.000000000000000000, 44.00000000000000711 ) ) ;
#275 = DIRECTION ( 'NONE',  ( -1.000000000000000000, 0.000000000000000000, 0.000000000000000000 ) ) ;
#276 = VECTOR ( 'NONE', #3647, 1000.000000000000000 ) ;
#277 = EDGE_LOOP ( 'NONE', ( #2977, #5435, #3484, #3552 ) ) ;
#278 = CARTESIAN_POINT ( 'NONE',  ( 0.000000000000000000, 0.000000000000000000, -115.0000000000000000 ) ) ;
#279 = ORIENTED_EDGE ( 'NONE', *, *, #1801, .T. ) ;
#280 = VECTOR ( 'NONE', #5453, 1000.000000000000000 ) ;
#281 = CARTESIAN_POINT ( 'NONE',  ( -13.41482486054668044, 26.39531364385071299, 5.999999999999990230 ) ) ;
#282 = APPLICATION_PROTOCOL_DEFINITION ( 'draft international standard', 'automotive_design', 1998, #1178 ) ;
#283 = CARTESIAN_POINT ( 'NONE',  ( 10.37037532854004418, -20.54332595864094202, 6.688011403969689184 ) ) ;
#284 = CIRCLE ( 'NONE', #4395, 22.00000000000000000 ) ;
#285 = ORIENTED_EDGE ( 'NONE', *, *, #6012, .F. ) ;
#286 = CYLINDRICAL_SURFACE ( 'NONE', #1017, 45.99999999999997868 ) ;
#287 = ORIENTED_EDGE ( 'NONE', *, *, #1156, .F. ) ;
#288 = VECTOR ( 'NONE', #565, 1000.000000000000000 ) ;
#289 = DIRECTION ( 'NONE',  ( -1.000000000000000000, 0.000000000000000000, 0.000000000000000000 ) ) ;
#290 = CARTESIAN_POINT ( 'NONE',  ( 0.000000000000000000, 0.000000000000000000, 0.000000000000000000 ) ) ;
#291 = DIRECTION ( 'NONE',  ( -0.000000000000000000, -0.000000000000000000, -1.000000000000000000 ) ) ;
#292 = CARTESIAN_POINT ( 'NONE',  ( 44.00000000000000000, -13.41640786499873705, -45.00000000000000000 ) ) ;
#293 = AXIS2_PLACEMENT_3D ( 'NONE', #3650, #5626, #3015 ) ;
#294 = AXIS2_PLACEMENT_3D ( 'NONE', #2245, #5189, #5257 ) ;
#295 = CARTESIAN_POINT ( 'NONE',  ( -2.426466830553623222, -24.88612820222272148, 38.88851386838337731 ) ) ;
#296 = ORIENTED_EDGE ( 'NONE', *, *, #3074, .T. ) ;
#297 = CARTESIAN_POINT ( 'NONE',  ( -10.37037532854004418, 20.54332595864094202, 6.688011403969689184 ) ) ;
#298 = ORIENTED_EDGE ( 'NONE', *, *, #69, .T. ) ;
#299 = EDGE_CURVE ( 'NONE', #686, #51, #842, .T. ) ;
#300 = CARTESIAN_POINT ( 'NONE',  ( 7.246617758453442804, 23.92680898849839721, 29.82624669321133126 ) ) ;
#301 = CARTESIAN_POINT ( 'NONE',  ( 44.43364355155687662, -29.42304313293534790, -180.0000000000000000 ) ) ;
#302 = AXIS2_PLACEMENT_3D ( 'NONE', #35, #5903, #5416 ) ;
#303 = CARTESIAN_POINT ( 'NONE',  ( 0.000000000000000000, 120.0000000000000000, -4.000000000000000000 ) ) ;
#304 = CARTESIAN_POINT ( 'NONE',  ( 7.306265819825862096, -23.90859775135293219, 30.06340984243352921 ) ) ;
#305 = EDGE_CURVE ( 'NONE', #5346, #4831, #1115, .T. ) ;
#306 = VERTEX_POINT ( 'NONE', #1172 ) ;
#307 = CARTESIAN_POINT ( 'NONE',  ( -3.336113272159680676, 24.78061407909199687, 25.03989924742864304 ) ) ;
#308 = VECTOR ( 'NONE', #2366, 1000.000000000000000 ) ;
#309 = VECTOR ( 'NONE', #6106, 1000.000000000000000 ) ;
#310 = DIRECTION ( 'NONE',  ( 1.000000000000000000, 0.000000000000000000, 0.000000000000000000 ) ) ;
#311 = CIRCLE ( 'NONE', #916, 25.00000000000000000 ) ;
#312 = DIRECTION ( 'NONE',  ( -0.000000000000000000, 0.000000000000000000, -1.000000000000000000 ) ) ;
#313 = EDGE_CURVE ( 'NONE', #2336, #4284, #725, .T. ) ;
#314 = FACE_BOUND ( 'NONE', #5611, .T. ) ;
#315 = EDGE_CURVE ( 'NONE', #1906, #997, #247, .T. ) ;
#316 = AXIS2_PLACEMENT_3D ( 'NONE', #4448, #5394, #4967 ) ;
#317 = ORIENTED_EDGE ( 'NONE', *, *, #272, .T. ) ;
#318 = CARTESIAN_POINT ( 'NONE',  ( -8.000000000000021316, 1.481987083124922376E-15, 12.00000000000000000 ) ) ;
#319 = ORIENTED_EDGE ( 'NONE', *, *, #4152, .T. ) ;
#320 = DIRECTION ( 'NONE',  ( -0.000000000000000000, -0.000000000000000000, 1.000000000000000000 ) ) ;
#321 = AXIS2_PLACEMENT_3D ( 'NONE', #133, #3087, #5016 ) ;
#322 = EDGE_CURVE ( 'NONE', #5682, #117, #4160, .T. ) ;
#323 = CARTESIAN_POINT ( 'NONE',  ( -4.378668635177231927, -22.59503479412315485, 9.474032806803469597 ) ) ;
#324 = ORIENTED_EDGE ( 'NONE', *, *, #5982, .T. ) ;
#325 = CARTESIAN_POINT ( 'NONE',  ( -19.00000000000000000, 2.326828918379970970E-15, -248.0000000000000000 ) ) ;
#326 = ORIENTED_EDGE ( 'NONE', *, *, #3688, .T. ) ;
#327 = EDGE_CURVE ( 'NONE', #4956, #1995, #4828, .T. ) ;
#328 = VECTOR ( 'NONE', #3380, 1000.000000000000000 ) ;
#329 = AXIS2_PLACEMENT_3D ( 'NONE', #4721, #320, #1790 ) ;
#330 = SHAPE_REPRESENTATION_RELATIONSHIP ( 'NONE' , 'NONE' ,  #5199, #2789 ) ;
#331 = DIRECTION ( 'NONE',  ( -0.000000000000000000, -0.000000000000000000, -1.000000000000000000 ) ) ;
#332 = DIRECTION ( 'NONE',  ( 0.000000000000000000, 1.740526192617802767E-17, -1.000000000000000000 ) ) ;
#333 = DIRECTION ( 'NONE',  ( -1.000000000000000000, 0.000000000000000000, 0.000000000000000000 ) ) ;
#334 = ORIENTED_EDGE ( 'NONE', *, *, #1705, .F. ) ;
#335 =( NAMED_UNIT ( * ) PLANE_ANGLE_UNIT ( ) SI_UNIT ( $, .RADIAN. ) );
#336 = VERTEX_POINT ( 'NONE', #3204 ) ;
#337 = CARTESIAN_POINT ( 'NONE',  ( 7.102515314070983798, 23.96997983984566361, 29.35314634237167297 ) ) ;
#338 = CARTESIAN_POINT ( 'NONE',  ( 59.99991398172927859, 8.702630963089024930E-17, 276.0000000000000000 ) ) ;
#339 = CARTESIAN_POINT ( 'NONE',  ( 132.0000000000000000, 69.00000000000000000, 0.000000000000000000 ) ) ;
#340 = CARTESIAN_POINT ( 'NONE',  ( 7.059265739357024394, -21.89000174688035827, 29.23188816227238362 ) ) ;
#341 = VERTEX_POINT ( 'NONE', #281 ) ;
#342 = ORIENTED_EDGE ( 'NONE', *, *, #3066, .F. ) ;
#343 = CARTESIAN_POINT ( 'NONE',  ( -0.4915545007834206670, 24.99637963107063499, 39.26296923598712851 ) ) ;
#344 = DIRECTION ( 'NONE',  ( 1.000000000000000000, 0.000000000000000000, 0.000000000000000000 ) ) ;
#345 = CARTESIAN_POINT ( 'NONE',  ( 265.0000000000000000, 0.000000000000000000, 110.0000000000000000 ) ) ;
#346 = FACE_OUTER_BOUND ( 'NONE', #5806, .T. ) ;
#347 = EDGE_LOOP ( 'NONE', ( #3523, #3999, #1718, #5180 ) ) ;
#348 = ORIENTED_EDGE ( 'NONE', *, *, #5467, .F. ) ;
#349 = ORIENTED_EDGE ( 'NONE', *, *, #5310, .T. ) ;
#350 = AXIS2_PLACEMENT_3D ( 'NONE', #4646, #3102, #2588 ) ;
#351 = CARTESIAN_POINT ( 'NONE',  ( 0.000000000000000000, 0.000000000000000000, 0.000000000000000000 ) ) ;
#352 = CARTESIAN_POINT ( 'NONE',  ( 3.009099790203600300, -22.80648947684007410, 9.749155414846011780 ) ) ;
#353 = DIRECTION ( 'NONE',  ( -1.000000000000000000, 0.000000000000000000, 0.000000000000000000 ) ) ;
#354 = EDGE_LOOP ( 'NONE', ( #837, #2657 ) ) ;
#355 = DIRECTION ( 'NONE',  ( -1.000000000000000000, 0.000000000000000000, 0.000000000000000000 ) ) ;
#356 = ORIENTED_EDGE ( 'NONE', *, *, #2582, .T. ) ;
#357 = FILL_AREA_STYLE_COLOUR ( '', #68 ) ;
#358 = EDGE_CURVE ( 'NONE', #4881, #53, #311, .T. ) ;
#359 = DIRECTION ( 'NONE',  ( 0.000000000000000000, 0.000000000000000000, 1.000000000000000000 ) ) ;
#360 = DIRECTION ( 'NONE',  ( -0.000000000000000000, -0.000000000000000000, -1.000000000000000000 ) ) ;
#361 = CARTESIAN_POINT ( 'NONE',  ( -4.953190041214019068, -24.50516424074860922, 26.13799397941500757 ) ) ;
#362 = ORIENTED_EDGE ( 'NONE', *, *, #5906, .F. ) ;
#363 = EDGE_CURVE ( 'NONE', #4783, #2333, #5736, .T. ) ;
#364 = DIRECTION ( 'NONE',  ( -0.000000000000000000, -0.000000000000000000, -1.000000000000000000 ) ) ;
#365 = MANIFOLD_SOLID_BREP ( 'Cut-Extrude4', #5984 ) ;
#366 = FACE_OUTER_BOUND ( 'NONE', #4514, .T. ) ;
#367 = DIRECTION ( 'NONE',  ( -0.000000000000000000, -0.000000000000000000, -1.000000000000000000 ) ) ;
#368 = DIRECTION ( 'NONE',  ( 0.000000000000000000, 0.000000000000000000, -1.000000000000000000 ) ) ;
#369 = CARTESIAN_POINT ( 'NONE',  ( 7.450717329638294473, -23.86413627455948117, 32.76425935539838008 ) ) ;
#370 = ORIENTED_EDGE ( 'NONE', *, *, #6217, .T. ) ;
#371 = VERTEX_POINT ( 'NONE', #5182 ) ;
#372 = CARTESIAN_POINT ( 'NONE',  ( -7.499773188859400364, 23.84855136421925437, 31.27916535100971274 ) ) ;
#373 = DIRECTION ( 'NONE',  ( 0.000000000000000000, 0.000000000000000000, 1.000000000000000000 ) ) ;
#374 = DIRECTION ( 'NONE',  ( 1.000000000000000000, 0.000000000000000000, 0.000000000000000000 ) ) ;
#375 = AXIS2_PLACEMENT_3D ( 'NONE', #3837, #2921, #5808 ) ;
#376 = CARTESIAN_POINT ( 'NONE',  ( 0.000000000000000000, 0.000000000000000000, 0.000000000000000000 ) ) ;
#377 = AXIS2_PLACEMENT_3D ( 'NONE', #2646, #5558, #3130 ) ;
#378 = ORIENTED_EDGE ( 'NONE', *, *, #1539, .F. ) ;
#379 = ORIENTED_EDGE ( 'NONE', *, *, #464, .T. ) ;
#380 = ORIENTED_EDGE ( 'NONE', *, *, #582, .T. ) ;
#381 = DIRECTION ( 'NONE',  ( -0.000000000000000000, -0.000000000000000000, -1.000000000000000000 ) ) ;
#382 = CIRCLE ( 'NONE', #5939, 90.00000000000319744 ) ;
#383 = AXIS2_PLACEMENT_3D ( 'NONE', #932, #2408, #6282 ) ;
#384 = CARTESIAN_POINT ( 'NONE',  ( 14.00000000000000000, 14.00000000000000000, 110.0000000000000000 ) ) ;
#385 = PLANE ( 'NONE',  #1235 ) ;
#386 = ORIENTED_EDGE ( 'NONE', *, *, #5059, .F. ) ;
#387 = ADVANCED_FACE ( 'NONE', ( #4260 ), #5210, .T. ) ;
#388 = CARTESIAN_POINT ( 'NONE',  ( 0.000000000000000000, 25.00000000000000000, -30.00000000000000000 ) ) ;
#389 =( GEOMETRIC_REPRESENTATION_CONTEXT ( 3 ) GLOBAL_UNCERTAINTY_ASSIGNED_CONTEXT ( ( #5158 ) ) GLOBAL_UNIT_ASSIGNED_CONTEXT ( ( #5187, #2278, #1180 ) ) REPRESENTATION_CONTEXT ( 'NONE', 'WORKASPACE' ) );
#390 = EDGE_CURVE ( 'NONE', #5661, #673, #5569, .T. ) ;
#391 = DIRECTION ( 'NONE',  ( -1.000000000000000000, 0.000000000000000000, 0.000000000000000000 ) ) ;
#392 = DIRECTION ( 'NONE',  ( -0.000000000000000000, -0.000000000000000000, -1.000000000000000000 ) ) ;
#393 = CARTESIAN_POINT ( 'NONE',  ( 9.184177739184520255E-16, -25.00000000000000000, 39.27501000028010480 ) ) ;
#394 = VERTEX_POINT ( 'NONE', #2235 ) ;
#395 = EDGE_CURVE ( 'NONE', #5724, #1881, #5157, .T. ) ;
#396 = CARTESIAN_POINT ( 'NONE',  ( 0.000000000000000000, 0.000000000000000000, -65.00000000000000000 ) ) ;
#397 = AXIS2_PLACEMENT_3D ( 'NONE', #5759, #4256, #374 ) ;
#398 = CARTESIAN_POINT ( 'NONE',  ( 8.000000000000021316, 2.721075280251214820E-15, 1.999999999999986233 ) ) ;
#399 = CARTESIAN_POINT ( 'NONE',  ( 0.000000000000000000, 0.000000000000000000, 48.00000000000000000 ) ) ;
#400 = AXIS2_PLACEMENT_3D ( 'NONE', #2031, #1061, #2896 ) ;
#401 = ADVANCED_FACE ( 'NONE', ( #6178 ), #5246, .T. ) ;
#402 = CARTESIAN_POINT ( 'NONE',  ( 0.000000000000000000, -25.00000000000000000, 0.000000000000000000 ) ) ;
#403 = CARTESIAN_POINT ( 'NONE',  ( 6.830924868230229485, -24.04887075291642873, 34.88135594814354334 ) ) ;
#404 = ORIENTED_EDGE ( 'NONE', *, *, #2795, .F. ) ;
#405 = EDGE_CURVE ( 'NONE', #6324, #2388, #3760, .T. ) ;
#406 = CIRCLE ( 'NONE', #2964, 17.00000000000000000 ) ;
#407 = ORIENTED_EDGE ( 'NONE', *, *, #5272, .F. ) ;
#408 = CARTESIAN_POINT ( 'NONE',  ( -6.096488593930904365, 24.24566755320543976, 36.15017996222949392 ) ) ;
#409 = CARTESIAN_POINT ( 'NONE',  ( 42.00000000000000000, 69.00000000000000000, 110.0000000000000000 ) ) ;
#410 = CARTESIAN_POINT ( 'NONE',  ( 16.23652742703164620, 37.28747423195200383, 0.000000000000000000 ) ) ;
#411 = VECTOR ( 'NONE', #4080, 1000.000000000000000 ) ;
#412 = LINE ( 'NONE', #3355, #3285 ) ;
#413 = EDGE_LOOP ( 'NONE', ( #6163, #678, #2072, #1728, #5455, #5735 ) ) ;
#414 = VERTEX_POINT ( 'NONE', #4884 ) ;
#415 = AXIS2_PLACEMENT_3D ( 'NONE', #376, #1368, #2905 ) ;
#416 = AXIS2_PLACEMENT_3D ( 'NONE', #2228, #2708, #5621 ) ;
#417 = CARTESIAN_POINT ( 'NONE',  ( -3.122849337825752983E-15, -17.00000000000000000, 281.0000000000000000 ) ) ;
#418 = DIRECTION ( 'NONE',  ( 1.852483853906148040E-16, 1.000000000000000000, 0.000000000000000000 ) ) ;
#419 = AXIS2_PLACEMENT_3D ( 'NONE', #4172, #1605, #6062 ) ;
#420 = DIRECTION ( 'NONE',  ( 0.000000000000000000, 0.000000000000000000, 1.000000000000000000 ) ) ;
#421 = ORIENTED_EDGE ( 'NONE', *, *, #4564, .T. ) ;
#422 = AXIS2_PLACEMENT_3D ( 'NONE', #4770, #2723, #5320 ) ;
#423 = CARTESIAN_POINT ( 'NONE',  ( 17.00000000000000000, 2.081899558550500280E-15, -180.0000000000000000 ) ) ;
#424 = CARTESIAN_POINT ( 'NONE',  ( -5.575863217335945698, -22.31445838370337853, 26.75407420319146823 ) ) ;
#425 = DIRECTION ( 'NONE',  ( 1.000000000000000000, 0.000000000000000000, 0.000000000000000000 ) ) ;
#426 = CARTESIAN_POINT ( 'NONE',  ( 12.41746183822997551, 30.39531364385071655, 9.999999999999991118 ) ) ;
#427 = VERTEX_POINT ( 'NONE', #3878 ) ;
#428 = DIRECTION ( 'NONE',  ( 0.000000000000000000, 0.000000000000000000, 1.000000000000000000 ) ) ;
#429 = CARTESIAN_POINT ( 'NONE',  ( 0.9889208576060609657, 24.98510605705583743, 24.32423630022272576 ) ) ;
#430 = CARTESIAN_POINT ( 'NONE',  ( 0.000000000000000000, 0.000000000000000000, 50.00000000000000711 ) ) ;
#431 = CARTESIAN_POINT ( 'NONE',  ( 7.443729366988918004E-21, -23.00000000000000000, 24.27501000028010125 ) ) ;
#432 = ORIENTED_EDGE ( 'NONE', *, *, #4266, .F. ) ;
#433 = FACE_OUTER_BOUND ( 'NONE', #246, .T. ) ;
#434 = VERTEX_POINT ( 'NONE', #1372 ) ;
#435 = CARTESIAN_POINT ( 'NONE',  ( -5.723282545231354490, 22.27700230555918992, 36.62722877095559681 ) ) ;
#436 = CIRCLE ( 'NONE', #2788, 46.00000000000000000 ) ;
#437 = CARTESIAN_POINT ( 'NONE',  ( 0.000000000000000000, 0.000000000000000000, 39.00000000000001421 ) ) ;
#438 = DIRECTION ( 'NONE',  ( -0.000000000000000000, -0.000000000000000000, -1.000000000000000000 ) ) ;
#439 = CARTESIAN_POINT ( 'NONE',  ( 13.14183123006952947, -39.58265509608667543, -49.99999999999999289 ) ) ;
#440 = ORIENTED_EDGE ( 'NONE', *, *, #1522, .T. ) ;
#441 = EDGE_LOOP ( 'NONE', ( #370, #4762, #5262, #4318 ) ) ;
#442 = LINE ( 'NONE', #6275, #1455 ) ;
#443 = ITEM_DEFINED_TRANSFORMATION ( 'NONE', 'NONE', #6047,  #6349 ) ;
#444 = DIRECTION ( 'NONE',  ( -0.000000000000000000, -0.000000000000000000, -1.000000000000000000 ) ) ;
#445 = AXIS2_PLACEMENT_3D ( 'NONE', #503, #6298, #3844 ) ;
#446 = CARTESIAN_POINT ( 'NONE',  ( -0.8363506376998798286, -25.00098981342394922, 10.00139094947510721 ) ) ;
#447 = ORIENTED_EDGE ( 'NONE', *, *, #662, .T. ) ;
#448 = DIRECTION ( 'NONE',  ( 0.000000000000000000, 0.000000000000000000, -1.000000000000000000 ) ) ;
#449 =( NAMED_UNIT ( * ) PLANE_ANGLE_UNIT ( ) SI_UNIT ( $, .RADIAN. ) );
#450 = CARTESIAN_POINT ( 'NONE',  ( 7.443729366988918004E-21, -23.00000000000000000, 24.27501000028010125 ) ) ;
#451 = DIRECTION ( 'NONE',  ( 0.000000000000000000, 0.000000000000000000, 1.000000000000000000 ) ) ;
#452 = CARTESIAN_POINT ( 'NONE',  ( 14.00000000000000000, 0.000000000000000000, 0.000000000000000000 ) ) ;
#453 = VERTEX_POINT ( 'NONE', #2946 ) ;
#454 = DIRECTION ( 'NONE',  ( -0.000000000000000000, -0.000000000000000000, -1.000000000000000000 ) ) ;
#455 = PLANE ( 'NONE',  #375 ) ;
#456 = CARTESIAN_POINT ( 'NONE',  ( -13.05910636442709993, 27.77388734089488054, 2.967234880352094706 ) ) ;
#457 = FACE_BOUND ( 'NONE', #4717, .T. ) ;
#458 = LINE ( 'NONE', #232, #5970 ) ;
#459 = EDGE_LOOP ( 'NONE', ( #5395, #324, #5477, #2014 ) ) ;
#460 = CARTESIAN_POINT ( 'NONE',  ( 16.99999999999999645, -24.99999999999999645, -160.0000000000000000 ) ) ;
#461 = CARTESIAN_POINT ( 'NONE',  ( -8.000000000000007105, 72.93807001241029297, 0.000000000000000000 ) ) ;
#462 = CARTESIAN_POINT ( 'NONE',  ( -2.869322346082823660, 22.82391999846087316, 38.71877048136666843 ) ) ;
#463 = EDGE_CURVE ( 'NONE', #2750, #4432, #4528, .T. ) ;
#464 = EDGE_CURVE ( 'NONE', #6000, #1209, #1438, .T. ) ;
#465 = FACE_OUTER_BOUND ( 'NONE', #4295, .T. ) ;
#466 = ADVANCED_FACE ( 'NONE', ( #4852 ), #5892, .T. ) ;
#467 = CARTESIAN_POINT ( 'NONE',  ( 19.00000000000000000, 0.000000000000000000, -240.0000000000000000 ) ) ;
#468 = DIRECTION ( 'NONE',  ( 0.000000000000000000, 0.000000000000000000, 1.000000000000000000 ) ) ;
#469 = ORIENTED_EDGE ( 'NONE', *, *, #2472, .F. ) ;
#470 = ORIENTED_EDGE ( 'NONE', *, *, #1913, .T. ) ;
#471 = ORIENTED_EDGE ( 'NONE', *, *, #1342, .T. ) ;
#472 = ADVANCED_FACE ( 'NONE', ( #5860 ), #5405, .F. ) ;
#473 = EDGE_CURVE ( 'NONE', #4999, #4629, #2884, .T. ) ;
#474 = ORIENTED_EDGE ( 'NONE', *, *, #5909, .T. ) ;
#475 = LINE ( 'NONE', #892, #5466 ) ;
#476 = AXIS2_PLACEMENT_3D ( 'NONE', #5538, #5967, #2537 ) ;
#477 = CONTEXT_DEPENDENT_SHAPE_REPRESENTATION ( #4557, #4091 ) ;
#478 = CARTESIAN_POINT ( 'NONE',  ( 25.00000000000000000, 3.061616997868383043E-15, 41.00000000000000000 ) ) ;
#479 = VECTOR ( 'NONE', #2555, 1000.000000000000000 ) ;
#480 = CARTESIAN_POINT ( 'NONE',  ( 6.500000000000000000, 0.000000000000000000, 1.000000000000000888 ) ) ;
#481 = ORIENTED_EDGE ( 'NONE', *, *, #1052, .T. ) ;
#482 = EDGE_CURVE ( 'NONE', #1816, #1146, #442, .T. ) ;
#483 = EDGE_CURVE ( 'NONE', #43, #3426, #961, .T. ) ;
#484 = CARTESIAN_POINT ( 'NONE',  ( 0.000000000000000000, 0.000000000000000000, 12.00000000000000000 ) ) ;
#485 = AXIS2_PLACEMENT_3D ( 'NONE', #747, #4694, #6145 ) ;
#486 =( LENGTH_UNIT ( ) NAMED_UNIT ( * ) SI_UNIT ( .MILLI., .METRE. ) );
#487 = LINE ( 'NONE', #5352, #1768 ) ;
#488 = DIRECTION ( 'NONE',  ( -1.836970198721029194E-16, -1.000000000000000000, 0.000000000000000000 ) ) ;
#489 = CARTESIAN_POINT ( 'NONE',  ( 17.00000000000000000, 2.081899558550500280E-15, -175.0000000000000000 ) ) ;
#490 = EDGE_LOOP ( 'NONE', ( #790, #2520, #3675, #298, #2628, #5964 ) ) ;
#491 = CARTESIAN_POINT ( 'NONE',  ( 2.012341796004660122, 19.89850447888114005, 39.00000000000001421 ) ) ;
#492 = AXIS2_PLACEMENT_3D ( 'NONE', #3372, #5351, #933 ) ;
#493 = CARTESIAN_POINT ( 'NONE',  ( 0.000000000000000000, 120.0000000000000000, -4.000000000000000000 ) ) ;
#494 = PLANE ( 'NONE',  #4742 ) ;
#495 = CARTESIAN_POINT ( 'NONE',  ( -13.15471301119415237, 27.39842886758932039, 3.337628543836458572 ) ) ;
#496 = AXIS2_PLACEMENT_3D ( 'NONE', #5868, #1446, #5317 ) ;
#497 = CARTESIAN_POINT ( 'NONE',  ( 262.0000000000000000, 68.99999999999997158, 110.0000000000000000 ) ) ;
#498 = EDGE_LOOP ( 'NONE', ( #6199, #5221 ) ) ;
#499 = EDGE_CURVE ( 'NONE', #2855, #4961, #475, .T. ) ;
#500 = CARTESIAN_POINT ( 'NONE',  ( 5.608440128082920140, 22.30969483029271672, 9.098285821462422263 ) ) ;
#501 = CARTESIAN_POINT ( 'NONE',  ( 12.84201764556569714, 28.64001483306502038, 9.603681688880103096 ) ) ;
#502 =( REPRESENTATION_RELATIONSHIP ('NONE','NONE', #632, #1490 ) REPRESENTATION_RELATIONSHIP_WITH_TRANSFORMATION ( #443 )SHAPE_REPRESENTATION_RELATIONSHIP( ) );
#503 = CARTESIAN_POINT ( 'NONE',  ( 0.000000000000000000, 0.000000000000000000, 47.00000000000000711 ) ) ;
#504 = CIRCLE ( 'NONE', #397, 22.00000000000000000 ) ;
#505 = DIRECTION ( 'NONE',  ( 0.000000000000000000, 0.000000000000000000, -1.000000000000000000 ) ) ;
#506 = ADVANCED_FACE ( 'NONE', ( #3791 ), #1826, .F. ) ;
#507 = CYLINDRICAL_SURFACE ( 'NONE', #605, 22.67164836619066648 ) ;
#508 = DIRECTION ( 'NONE',  ( -0.000000000000000000, -0.000000000000000000, -1.000000000000000000 ) ) ;
#509 = ORIENTED_EDGE ( 'NONE', *, *, #679, .T. ) ;
#510 = AXIS2_PLACEMENT_3D ( 'NONE', #2170, #6108, #5525 ) ;
#511 = ORIENTED_EDGE ( 'NONE', *, *, #8, .F. ) ;
#512 = EDGE_LOOP ( 'NONE', ( #5919, #649, #3464, #3350, #1652, #1767, #4821, #6182, #378 ) ) ;
#513 = EDGE_LOOP ( 'NONE', ( #2554, #1774, #6009, #4484, #4684, #1934, #3854, #3458 ) ) ;
#514 = ADVANCED_FACE ( 'NONE', ( #1956 ), #5797, .T. ) ;
#515 = DIRECTION ( 'NONE',  ( -0.000000000000000000, -0.000000000000000000, 1.000000000000000000 ) ) ;
#516 = LINE ( 'NONE', #640, #2756 ) ;
#517 = EDGE_CURVE ( 'NONE', #51, #146, #2675, .T. ) ;
#518 = PLANE ( 'NONE',  #2853 ) ;
#519 = ORIENTED_EDGE ( 'NONE', *, *, #1522, .F. ) ;
#520 = TOROIDAL_SURFACE ( 'NONE', #621, 6.500000000000000000, 1.000000000000000000 ) ;
#521 = EDGE_CURVE ( 'NONE', #1518, #997, #1473, .T. ) ;
#522 = CARTESIAN_POINT ( 'NONE',  ( 265.0000000000000000, 0.000000000000000000, 0.000000000000000000 ) ) ;
#523 = DIRECTION ( 'NONE',  ( 0.9999999999999998890, 2.669069574419021450E-17, -2.824691619778199685E-21 ) ) ;
#524 = CARTESIAN_POINT ( 'NONE',  ( 15.99408614349810698, -19.21429697996681440, 0.000000000000000000 ) ) ;
#525 = CYLINDRICAL_SURFACE ( 'NONE', #2568, 21.00000000000000355 ) ;
#526 = EDGE_LOOP ( 'NONE', ( #3915, #2358, #2129, #2824 ) ) ;
#527 = DIRECTION ( 'NONE',  ( -0.000000000000000000, -0.000000000000000000, -1.000000000000000000 ) ) ;
#528 = AXIS2_PLACEMENT_3D ( 'NONE', #2486, #3029, #1942 ) ;
#529 = EDGE_CURVE ( 'NONE', #5958, #3408, #5766, .T. ) ;
#530 = DIRECTION ( 'NONE',  ( -0.000000000000000000, -0.000000000000000000, 1.000000000000000000 ) ) ;
#531 = CARTESIAN_POINT ( 'NONE',  ( 5.958576596270775738, 24.28117850353844531, 27.19366677815228783 ) ) ;
#532 = CIRCLE ( 'NONE', #4010, 22.00000000000000000 ) ;
#533 = CARTESIAN_POINT ( 'NONE',  ( 6.500000000000005329, 120.0000000000000000, 16.00000000000000000 ) ) ;
#534 = EDGE_LOOP ( 'NONE', ( #3667, #4259, #1985, #3531 ) ) ;
#535 =( NAMED_UNIT ( * ) PLANE_ANGLE_UNIT ( ) SI_UNIT ( $, .RADIAN. ) );
#536 = CARTESIAN_POINT ( 'NONE',  ( 12.89883946988004659, 28.41146683342871881, 9.483046795230265502 ) ) ;
#537 = CARTESIAN_POINT ( 'NONE',  ( 0.000000000000000000, 25.00000000000000000, -225.0000000000000000 ) ) ;
#538 = AXIS2_PLACEMENT_3D ( 'NONE', #4344, #1903, #5392 ) ;
#539 = CYLINDRICAL_SURFACE ( 'NONE', #6196, 89.87058297576894006 ) ;
#540 = CARTESIAN_POINT ( 'NONE',  ( -3.122849337825752983E-15, -17.00000000000000000, 301.0000000000000568 ) ) ;
#541 = CYLINDRICAL_SURFACE ( 'NONE', #6, 72.49991987048068154 ) ;
#542 = VERTEX_POINT ( 'NONE', #5283 ) ;
#543 = EDGE_LOOP ( 'NONE', ( #3781, #3174, #5864, #4593 ) ) ;
#544 = ORIENTED_EDGE ( 'NONE', *, *, #222, .T. ) ;
#545 = CIRCLE ( 'NONE', #4854, 23.00000000000000000 ) ;
#546 = DIRECTION ( 'NONE',  ( -0.000000000000000000, 0.000000000000000000, -1.000000000000000000 ) ) ;
#547 = DIRECTION ( 'NONE',  ( 0.000000000000000000, -1.000000000000000000, 0.000000000000000000 ) ) ;
#548 = EDGE_CURVE ( 'NONE', #647, #4703, #866, .T. ) ;
#549 = CARTESIAN_POINT ( 'NONE',  ( 2.201053925086813301, -24.90665284231784327, 9.868642342566223746 ) ) ;
#550 = ORIENTED_EDGE ( 'NONE', *, *, #4554, .F. ) ;
#551 = DIRECTION ( 'NONE',  ( 1.083164258625200090E-16, -1.000000000000000000, 3.008588357523847888E-23 ) ) ;
#552 = FACE_OUTER_BOUND ( 'NONE', #3126, .T. ) ;
#553 = DIRECTION ( 'NONE',  ( -0.000000000000000000, -0.000000000000000000, -1.000000000000000000 ) ) ;
#554 = VERTEX_POINT ( 'NONE', #4298 ) ;
#555 = CARTESIAN_POINT ( 'NONE',  ( -3.122849337825752983E-15, -17.00000000000000000, 281.0000000000000000 ) ) ;
#556 = CARTESIAN_POINT ( 'NONE',  ( 174.7835321302054865, 68.75545066608756883, 12.00000000000000000 ) ) ;
#557 = CARTESIAN_POINT ( 'NONE',  ( -6.500000000000000000, 0.000000000000000000, 12.00000000000000000 ) ) ;
#558 = CARTESIAN_POINT ( 'NONE',  ( -12.41746183823000393, 30.39531364385071299, 1.999999999999990008 ) ) ;
#559 = DIRECTION ( 'NONE',  ( 1.000000000000000000, 0.000000000000000000, 0.000000000000000000 ) ) ;
#560 = ORIENTED_EDGE ( 'NONE', *, *, #6031, .F. ) ;
#561 = FACE_OUTER_BOUND ( 'NONE', #3544, .T. ) ;
#562 = CARTESIAN_POINT ( 'NONE',  ( 0.000000000000000000, 0.000000000000000000, 41.00000000000000000 ) ) ;
#563 = CARTESIAN_POINT ( 'NONE',  ( -6.385057176062306716, 22.09706105569707191, 27.81520467947423114 ) ) ;
#564 = CARTESIAN_POINT ( 'NONE',  ( 0.000000000000000000, 0.000000000000000000, -20.00000000000000000 ) ) ;
#565 = DIRECTION ( 'NONE',  ( -0.000000000000000000, -0.000000000000000000, -1.000000000000000000 ) ) ;
#566 = DIRECTION ( 'NONE',  ( 1.000000000000000000, 0.000000000000000000, 0.000000000000000000 ) ) ;
#567 = ORIENTED_EDGE ( 'NONE', *, *, #125, .T. ) ;
#568 = ORIENTED_EDGE ( 'NONE', *, *, #5155, .T. ) ;
#569 = CIRCLE ( 'NONE', #3996, 17.00000000000000000 ) ;
#570 = ORIENTED_EDGE ( 'NONE', *, *, #988, .F. ) ;
#571 = CARTESIAN_POINT ( 'NONE',  ( 44.64065620456912598, 28.99954194078667413, -160.0000000000000284 ) ) ;
#572 = DIRECTION ( 'NONE',  ( -0.000000000000000000, -0.000000000000000000, 1.000000000000000000 ) ) ;
#573 = CYLINDRICAL_SURFACE ( 'NONE', #5444, 89.87058297576894006 ) ;
#574 = ORIENTED_EDGE ( 'NONE', *, *, #947, .F. ) ;
#575 = B_SPLINE_CURVE_WITH_KNOTS ( 'NONE', 3,
 ( #393, #6286, #1900, #2347, #295, #3772, #5741, #3216, #2380, #3743, #1839, #2282, #1873, #4243, #1314, #2246, #812, #4735, #5805, #6224, #877, #5703, #1772, #2316, #3311, #2823, #903, #6190, #5778, #5259, #845, #4308, #361, #2798, #3800, #4273, #1283, #5672, #3248, #5220, #5292, #3834 ),
 .UNSPECIFIED., .F., .F.,
 ( 4, 2, 2, 2, 2, 2, 2, 2, 2, 2, 2, 2, 2, 2, 2, 2, 2, 2, 2, 2, 4 ),
 ( 0.02358501416070326456, 0.02505868070871361541, 0.02653234725672396974, 0.02800601380473432406, 0.02947968035274467491, 0.03021651362674985727, 0.03095334690075503964, 0.03242701344876540437, 0.03390067999677577604, 0.03463751327078095493, 0.03537434654478614077, 0.03684801309279646386, 0.03758484636680162194, 0.03832167964080678696, 0.03979534618881712393, 0.04126901273682745397, 0.04200584601083262593, 0.04274267928483779788, 0.04421634583284814179, 0.04569001238085847877, 0.04716367892886881574 ),
 .UNSPECIFIED. ) ;
#576 = CONTEXT_DEPENDENT_SHAPE_REPRESENTATION ( #2169, #5137 ) ;
#577 = DIRECTION ( 'NONE',  ( -0.000000000000000000, -0.000000000000000000, 1.000000000000000000 ) ) ;
#578 = CARTESIAN_POINT ( 'NONE',  ( -6.497654244294650105, -22.06338186837085402, 35.52745571863555085 ) ) ;
#579 = EDGE_CURVE ( 'NONE', #5734, #4913, #1971, .T. ) ;
#580 = CARTESIAN_POINT ( 'NONE',  ( 0.000000000000000000, 76.99999716619419132, 281.0000000000000000 ) ) ;
#581 = ORIENTED_EDGE ( 'NONE', *, *, #6309, .F. ) ;
#582 = EDGE_CURVE ( 'NONE', #2231, #3044, #4224, .T. ) ;
#583 = FACE_BOUND ( 'NONE', #2042, .T. ) ;
#584 = FACE_OUTER_BOUND ( 'NONE', #5731, .T. ) ;
#585 = AXIS2_PLACEMENT_3D ( 'NONE', #4125, #6104, #5138 ) ;
#586 = DIRECTION ( 'NONE',  ( 1.000000000000000000, 0.000000000000000000, -0.000000000000000000 ) ) ;
#587 = AXIS2_PLACEMENT_3D ( 'NONE', #5409, #4922, #1833 ) ;
#588 = EDGE_CURVE ( 'NONE', #3260, #713, #5667, .T. ) ;
#589 = DIRECTION ( 'NONE',  ( -0.000000000000000000, -0.000000000000000000, 1.000000000000000000 ) ) ;
#590 = VERTEX_POINT ( 'NONE', #5560 ) ;
#591 = AXIS2_PLACEMENT_3D ( 'NONE', #5540, #4567, #168 ) ;
#592 = CARTESIAN_POINT ( 'NONE',  ( 15.63711455316257215, 16.87386736187478675, 0.7328676451471519693 ) ) ;
#593 = ORIENTED_EDGE ( 'NONE', *, *, #669, .F. ) ;
#594 = CARTESIAN_POINT ( 'NONE',  ( 3.065100562737908430, 22.79875969907089228, 24.91526600425119042 ) ) ;
#595 = EDGE_CURVE ( 'NONE', #5536, #1071, #2161, .T. ) ;
#596 =( GEOMETRIC_REPRESENTATION_CONTEXT ( 3 ) GLOBAL_UNCERTAINTY_ASSIGNED_CONTEXT ( ( #4277 ) ) GLOBAL_UNIT_ASSIGNED_CONTEXT ( ( #4212, #3630, #5802 ) ) REPRESENTATION_CONTEXT ( 'NONE', 'WORKASPACE' ) );
#597 = PRODUCT_RELATED_PRODUCT_CATEGORY ( 'part', '', ( #4667 ) ) ;
#598 = PLANE ( 'NONE',  #906 ) ;
#599 = DIRECTION ( 'NONE',  ( 1.000000000000000000, 0.000000000000000000, 0.000000000000000000 ) ) ;
#600 = ADVANCED_FACE ( 'NONE', ( #1021 ), #2589, .T. ) ;
#601 = ORIENTED_EDGE ( 'NONE', *, *, #363, .T. ) ;
#602 = VERTEX_POINT ( 'NONE', #1583 ) ;
#603 = ADVANCED_FACE ( 'NONE', ( #4032 ), #1136, .T. ) ;
#604 = EDGE_LOOP ( 'NONE', ( #4129, #2093, #1661, #1916 ) ) ;
#605 = AXIS2_PLACEMENT_3D ( 'NONE', #4876, #5431, #2069 ) ;
#606 = CARTESIAN_POINT ( 'NONE',  ( -19.00000000000000000, 0.000000000000000000, 23.00000000000000000 ) ) ;
#607 = EDGE_CURVE ( 'NONE', #1184, #5794, #4422, .T. ) ;
#608 = DIRECTION ( 'NONE',  ( 1.000000000000000000, 0.000000000000000000, 0.000000000000000000 ) ) ;
#609 = CARTESIAN_POINT ( 'NONE',  ( 0.000000000000000000, 0.000000000000000000, 39.00000000000001421 ) ) ;
#610 = CIRCLE ( 'NONE', #2025, 25.00000000000000000 ) ;
#611 = DIRECTION ( 'NONE',  ( 0.000000000000000000, -1.000000000000000000, 0.000000000000000000 ) ) ;
#612 = B_SPLINE_CURVE_WITH_KNOTS ( 'NONE', 3,
 ( #4261, #1894, #1864, #2817, #5344, #3852, #5730, #3825, #5798, #5379, #3329, #927, #6245, #5309, #1345, #5824, #1827, #5862 ),
 .UNSPECIFIED., .F., .F.,
 ( 4, 2, 2, 2, 2, 2, 2, 2, 4 ),
 ( 0.000000000000000000, 0.0007936035350328095447, 0.001587207070065619089, 0.002380810605098428526, 0.003174414140131238179, 0.003968017675164047832, 0.004761621210196857051, 0.005555224745229667138, 0.006348828280262476358 ),
 .UNSPECIFIED. ) ;
#613 = FACE_OUTER_BOUND ( 'NONE', #4079, .T. ) ;
#614 = ORIENTED_EDGE ( 'NONE', *, *, #5533, .T. ) ;
#615 = CARTESIAN_POINT ( 'NONE',  ( 96.31180517104780847, 82.87638965790611678, 281.2329880893516929 ) ) ;
#616 = DIRECTION ( 'NONE',  ( -0.000000000000000000, -0.000000000000000000, -1.000000000000000000 ) ) ;
#617 = FACE_OUTER_BOUND ( 'NONE', #3293, .T. ) ;
#618 = EDGE_LOOP ( 'NONE', ( #4862, #1550, #6154, #2406 ) ) ;
#619 = VECTOR ( 'NONE', #1169, 1000.000000000000000 ) ;
#620 = FACE_OUTER_BOUND ( 'NONE', #1678, .T. ) ;
#621 = AXIS2_PLACEMENT_3D ( 'NONE', #3961, #3985, #4962 ) ;
#622 = DIRECTION ( 'NONE',  ( 0.000000000000000000, -1.000000000000000000, -1.740526192617802767E-17 ) ) ;
#623 = DIRECTION ( 'NONE',  ( 1.000000000000000000, 0.000000000000000000, 0.000000000000000000 ) ) ;
#624 = VERTEX_POINT ( 'NONE', #2522 ) ;
#625 = PLANE ( 'NONE',  #1215 ) ;
#626 = CARTESIAN_POINT ( 'NONE',  ( 1.908796811648538206E-15, -20.00000000000000711, 39.27501000028011902 ) ) ;
#627 = CARTESIAN_POINT ( 'NONE',  ( -7.471932569767337995, 21.75248695045747382, 32.56440574765390039 ) ) ;
#628 = AXIS2_PLACEMENT_3D ( 'NONE', #2918, #553, #1542 ) ;
#629 = CARTESIAN_POINT ( 'NONE',  ( -14.34088693563092320, 20.48519421429849174, 2.767956487184815462 ) ) ;
#630 = VECTOR ( 'NONE', #6353, 1000.000000000000000 ) ;
#631 = CARTESIAN_POINT ( 'NONE',  ( -44.43364355155666345, 29.42304313293564988, -115.0000000000000000 ) ) ;
#632 = SHAPE_REPRESENTATION ( 'MAT-003', ( #671, #6250, #3468, #698, #4282, #496, #3264, #5222, #4074, #1306, #6047, #2436, #4914, #5743, #184, #2954 ), #155 ) ;
#633 = VERTEX_POINT ( 'NONE', #5954 ) ;
#634 = ORIENTED_EDGE ( 'NONE', *, *, #6210, .T. ) ;
#635 = VERTEX_POINT ( 'NONE', #123 ) ;
#636 = DIRECTION ( 'NONE',  ( 0.000000000000000000, -1.000000000000000000, 1.740526192617802767E-17 ) ) ;
#637 = AXIS2_PLACEMENT_3D ( 'NONE', #2186, #6003, #1185 ) ;
#638 = AXIS2_PLACEMENT_3D ( 'NONE', #1399, #3918, #2463 ) ;
#639 = FACE_OUTER_BOUND ( 'NONE', #3277, .T. ) ;
#640 = CARTESIAN_POINT ( 'NONE',  ( -17.05141243254543681, 0.000000000000000000, 12.00000000000000000 ) ) ;
#641 = CARTESIAN_POINT ( 'NONE',  ( 0.000000000000000000, 0.000000000000000000, 50.00000000000000711 ) ) ;
#642 = DIRECTION ( 'NONE',  ( 1.000000000000000000, 0.000000000000000000, 0.000000000000000000 ) ) ;
#643 = VERTEX_POINT ( 'NONE', #5521 ) ;
#644 = CONTEXT_DEPENDENT_SHAPE_REPRESENTATION ( #4135, #4142 ) ;
#645 = APPLICATION_PROTOCOL_DEFINITION ( 'draft international standard', 'automotive_design', 1998, #3361 ) ;
#646 = CARTESIAN_POINT ( 'NONE',  ( 174.7835321302054865, 68.75545066608756883, 12.00000000000000000 ) ) ;
#647 = VERTEX_POINT ( 'NONE', #152 ) ;
#648 = DIRECTION ( 'NONE',  ( 1.000000000000000000, 0.000000000000000000, 0.000000000000000000 ) ) ;
#649 = ORIENTED_EDGE ( 'NONE', *, *, #1493, .F. ) ;
#650 = DIRECTION ( 'NONE',  ( 0.000000000000000000, 0.000000000000000000, 1.000000000000000000 ) ) ;
#651 = CARTESIAN_POINT ( 'NONE',  ( 0.000000000000000000, 0.000000000000000000, 16.00000000000000000 ) ) ;
#652 = EDGE_LOOP ( 'NONE', ( #1890, #1670, #5992, #4403 ) ) ;
#653 = CARTESIAN_POINT ( 'NONE',  ( 0.000000000000000000, 0.000000000000000000, 23.77500997278103512 ) ) ;
#654 = VECTOR ( 'NONE', #851, 1000.000000000000000 ) ;
#655 = DIRECTION ( 'NONE',  ( -0.000000000000000000, -0.000000000000000000, -1.000000000000000000 ) ) ;
#656 = CARTESIAN_POINT ( 'NONE',  ( 6.381573266039188397, 22.09732860014628031, 35.72159715675526570 ) ) ;
#657 = PRODUCT ( 'MAT-003', 'MAT-003', '', ( #1594 ) ) ;
#658 = DIRECTION ( 'NONE',  ( 1.000000000000000000, 0.000000000000000000, 0.000000000000000000 ) ) ;
#659 = ORIENTED_EDGE ( 'NONE', *, *, #4580, .F. ) ;
#660 = EDGE_CURVE ( 'NONE', #4451, #1805, #3400, .T. ) ;
#661 = VERTEX_POINT ( 'NONE', #2983 ) ;
#662 = EDGE_CURVE ( 'NONE', #2268, #1338, #5885, .T. ) ;
#663 = DIRECTION ( 'NONE',  ( -0.000000000000000000, -0.000000000000000000, -1.000000000000000000 ) ) ;
#664 = EDGE_CURVE ( 'NONE', #1786, #1760, #2432, .T. ) ;
#665 = PRODUCT_DEFINITION_SHAPE ( 'NONE', 'NONE',  #6376 ) ;
#666 = CARTESIAN_POINT ( 'NONE',  ( 13.00793927997764321, 27.97619002235532903, 2.803925835876298844 ) ) ;
#667 = DIRECTION ( 'NONE',  ( 0.000000000000000000, -1.740526192617802767E-17, -1.000000000000000000 ) ) ;
#668 = DIRECTION ( 'NONE',  ( 0.000000000000000000, -0.000000000000000000, -1.000000000000000000 ) ) ;
#669 = EDGE_CURVE ( 'NONE', #394, #1346, #2015, .T. ) ;
#670 = ADVANCED_FACE ( 'NONE', ( #639 ), #3012, .T. ) ;
#671 = AXIS2_PLACEMENT_3D ( 'NONE', #2178, #3084, #2112 ) ;
#672 = LINE ( 'NONE', #5688, #3682 ) ;
#673 = VERTEX_POINT ( 'NONE', #2046 ) ;
#674 = DIRECTION ( 'NONE',  ( 1.000000000000000000, -1.418966808623772043E-15, 6.337409375514650371E-16 ) ) ;
#675 = DIRECTION ( 'NONE',  ( 1.000000000000000000, 3.576835832488757469E-15, 0.000000000000000000 ) ) ;
#676 = EDGE_LOOP ( 'NONE', ( #5922, #4982, #4164, #5464 ) ) ;
#677 = CARTESIAN_POINT ( 'NONE',  ( 0.000000000000000000, 0.000000000000000000, 281.0000000000000000 ) ) ;
#678 = ORIENTED_EDGE ( 'NONE', *, *, #2302, .T. ) ;
#679 = EDGE_CURVE ( 'NONE', #3152, #647, #1047, .T. ) ;
#680 = CARTESIAN_POINT ( 'NONE',  ( 0.000000000000000000, 120.0000000000000000, 16.00000000000000000 ) ) ;
#681 = CARTESIAN_POINT ( 'NONE',  ( -44.43364355155666345, 29.42304313293564988, -110.0000000000000000 ) ) ;
#682 = AXIS2_PLACEMENT_3D ( 'NONE', #37, #2481, #5417 ) ;
#683 = CARTESIAN_POINT ( 'NONE',  ( 0.000000000000000000, 0.000000000000000000, 15.00000000000000000 ) ) ;
#684 = AXIS2_PLACEMENT_3D ( 'NONE', #4760, #4654, #248 ) ;
#685 = DIRECTION ( 'NONE',  ( -0.000000000000000000, -0.000000000000000000, -1.000000000000000000 ) ) ;
#686 = VERTEX_POINT ( 'NONE', #3528 ) ;
#687 = DIRECTION ( 'NONE',  ( -0.000000000000000000, -0.000000000000000000, 1.000000000000000000 ) ) ;
#688 = CARTESIAN_POINT ( 'NONE',  ( -3.061616997868383043E-15, -25.00000000000000000, -160.0000000000000000 ) ) ;
#689 = CARTESIAN_POINT ( 'NONE',  ( 7.368286983821151992, 21.78790057683621129, 30.30389194166913569 ) ) ;
#690 = VECTOR ( 'NONE', #2330, 1000.000000000000000 ) ;
#691 = AXIS2_PLACEMENT_3D ( 'NONE', #5866, #899, #4889 ) ;
#692 = CARTESIAN_POINT ( 'NONE',  ( 9.287558414957929998, 23.21379839259252620, 7.388795739543629004 ) ) ;
#693 = ADVANCED_FACE ( 'NONE', ( #5493 ), #1074, .T. ) ;
#694 = CYLINDRICAL_SURFACE ( 'NONE', #2563, 17.00000000000000000 ) ;
#695 = ORIENTED_EDGE ( 'NONE', *, *, #3688, .F. ) ;
#696 = ORIENTED_EDGE ( 'NONE', *, *, #2847, .F. ) ;
#697 = DIRECTION ( 'NONE',  ( -0.000000000000000000, -0.000000000000000000, 1.000000000000000000 ) ) ;
#698 = AXIS2_PLACEMENT_3D ( 'NONE', #5384, #4368, #1929 ) ;
#699 = EDGE_CURVE ( 'NONE', #862, #6200, #5684, .T. ) ;
#700 = EDGE_CURVE ( 'NONE', #2130, #4703, #273, .T. ) ;
#701 = CARTESIAN_POINT ( 'NONE',  ( 6.500000000000000000, 130.6770782520313219, 0.000000000000000000 ) ) ;
#702 = DIRECTION ( 'NONE',  ( 0.000000000000000000, 0.000000000000000000, 1.000000000000000000 ) ) ;
#703 = CARTESIAN_POINT ( 'NONE',  ( 20.00000000000000000, 2.449293598294706513E-15, 51.00000000000002842 ) ) ;
#704 = CIRCLE ( 'NONE', #1097, 22.67164836619066648 ) ;
#705 = DIRECTION ( 'NONE',  ( -0.000000000000000000, -0.000000000000000000, -1.000000000000000000 ) ) ;
#706 = ORIENTED_EDGE ( 'NONE', *, *, #4636, .T. ) ;
#707 = EDGE_CURVE ( 'NONE', #2461, #2595, #1920, .T. ) ;
#708 = VECTOR ( 'NONE', #6348, 1000.000000000000000 ) ;
#709 = ITEM_DEFINED_TRANSFORMATION ( 'NONE', 'NONE', #496,  #6349 ) ;
#710 = CARTESIAN_POINT ( 'NONE',  ( 59.99991398172927859, -4.803852291625136032E-15, 5.000000000000004441 ) ) ;
#711 = ORIENTED_EDGE ( 'NONE', *, *, #938, .T. ) ;
#712 = DIRECTION ( 'NONE',  ( 0.000000000000000000, 0.000000000000000000, -1.000000000000000000 ) ) ;
#713 = VERTEX_POINT ( 'NONE', #1711 ) ;
#714 =( NAMED_UNIT ( * ) PLANE_ANGLE_UNIT ( ) SI_UNIT ( $, .RADIAN. ) );
#715 = CARTESIAN_POINT ( 'NONE',  ( -2.385244779468109755E-15, -1.040834085586084257E-14, -95.00000000000000000 ) ) ;
#716 = CYLINDRICAL_SURFACE ( 'NONE', #4439, 22.67164836619067714 ) ;
#717 = CIRCLE ( 'NONE', #200, 40.00000002749906258 ) ;
#718 = DIRECTION ( 'NONE',  ( -1.836970198721029194E-16, -1.000000000000000000, 0.000000000000000000 ) ) ;
#719 = CARTESIAN_POINT ( 'NONE',  ( 0.6815295361380621086, -19.99121204295638776, 39.25166565497248428 ) ) ;
#720 = ORIENTED_EDGE ( 'NONE', *, *, #5167, .T. ) ;
#721 = CARTESIAN_POINT ( 'NONE',  ( 1.798140372219934502, 22.93384243835984648, 9.914400014297026331 ) ) ;
#722 = AXIS2_PLACEMENT_3D ( 'NONE', #3398, #4786, #353 ) ;
#723 = PRODUCT_DEFINITION_SHAPE ( 'NONE', 'NONE',  #6369 ) ;
#724 = DIRECTION ( 'NONE',  ( 0.000000000000000000, -1.000000000000000000, -1.247733429937938623E-16 ) ) ;
#725 = CIRCLE ( 'NONE', #5871, 17.00000000000000000 ) ;
#726 = CARTESIAN_POINT ( 'NONE',  ( 82.00000000000001421, 69.00000000000000000, 110.0000000000000000 ) ) ;
#727 = AXIS2_PLACEMENT_3D ( 'NONE', #2541, #1976, #3964 ) ;
#728 = CARTESIAN_POINT ( 'NONE',  ( 2.450350183182338881, -22.87332759541404670, 38.87800362567253387 ) ) ;
#729 = ORIENTED_EDGE ( 'NONE', *, *, #3131, .T. ) ;
#730 = EDGE_LOOP ( 'NONE', ( #3326, #5717, #4359, #2877 ) ) ;
#731 = AXIS2_PLACEMENT_3D ( 'NONE', #3118, #4634, #1669 ) ;
#732 = CARTESIAN_POINT ( 'NONE',  ( -2.012341796004660122, -19.89850447888114005, 39.00000000000001421 ) ) ;
#733 = CARTESIAN_POINT ( 'NONE',  ( -22.00000000000000000, 0.000000000000000000, 44.00000000000000711 ) ) ;
#734 = DIRECTION ( 'NONE',  ( -0.000000000000000000, -0.000000000000000000, 1.000000000000000000 ) ) ;
#735 = AXIS2_PLACEMENT_3D ( 'NONE', #936, #3474, #1933 ) ;
#736 = FACE_OUTER_BOUND ( 'NONE', #1045, .T. ) ;
#737 = CARTESIAN_POINT ( 'NONE',  ( -8.000000000000007105, 72.93807001241029297, 12.00000000000000000 ) ) ;
#738 = VERTEX_POINT ( 'NONE', #793 ) ;
#739 =( GEOMETRIC_REPRESENTATION_CONTEXT ( 3 ) GLOBAL_UNCERTAINTY_ASSIGNED_CONTEXT ( ( #3662 ) ) GLOBAL_UNIT_ASSIGNED_CONTEXT ( ( #2204, #1242, #2172 ) ) REPRESENTATION_CONTEXT ( 'NONE', 'WORKASPACE' ) );
#740 = SURFACE_SIDE_STYLE ('',( #4757 ) ) ;
#741 = CARTESIAN_POINT ( 'NONE',  ( 11.01859089670589675, -20.20136408472527023, 6.200517937480644726 ) ) ;
#742 = ORIENTED_EDGE ( 'NONE', *, *, #1261, .T. ) ;
#743 = CARTESIAN_POINT ( 'NONE',  ( -44.00000000000000000, -13.41640786499873350, -45.00000000000000000 ) ) ;
#744 = ORIENTED_EDGE ( 'NONE', *, *, #3889, .T. ) ;
#745 = CIRCLE ( 'NONE', #3199, 25.00000000000000000 ) ;
#746 = ADVANCED_FACE ( 'NONE', ( #1268 ), #4618, .T. ) ;
#747 = CARTESIAN_POINT ( 'NONE',  ( 0.000000000000000000, 25.00000000000000000, -195.0000000000000000 ) ) ;
#748 = DIRECTION ( 'NONE',  ( -1.000000000000000000, 0.000000000000000000, 0.000000000000000000 ) ) ;
#749 = CARTESIAN_POINT ( 'NONE',  ( 14.00000000000000000, 14.00000000000000000, 110.0000000000000000 ) ) ;
#750 = DIRECTION ( 'NONE',  ( 1.000000000000000000, 0.000000000000000000, 0.000000000000000000 ) ) ;
#751 = ORIENTED_EDGE ( 'NONE', *, *, #944, .F. ) ;
#752 = EDGE_CURVE ( 'NONE', #673, #542, #2133, .T. ) ;
#753 = EDGE_CURVE ( 'NONE', #861, #3440, #3680, .T. ) ;
#754 = CARTESIAN_POINT ( 'NONE',  ( -8.997257985596670338, 21.18070524412206623, 7.578991052498396996 ) ) ;
#755 = ORIENTED_EDGE ( 'NONE', *, *, #988, .T. ) ;
#756 = DIRECTION ( 'NONE',  ( -1.000000000000000000, -0.000000000000000000, -0.000000000000000000 ) ) ;
#757 = CARTESIAN_POINT ( 'NONE',  ( -17.05141243254543681, -24.25762350764758679, 0.000000000000000000 ) ) ;
#758 = CARTESIAN_POINT ( 'NONE',  ( 0.8363506376998767200, 25.00098981342395277, 10.00139094947511076 ) ) ;
#759 = CARTESIAN_POINT ( 'NONE',  ( 7.411490251847205002, -21.77340291014862217, 33.00915547857365340 ) ) ;
#760 = VERTEX_POINT ( 'NONE', #5655 ) ;
#761 = ORIENTED_EDGE ( 'NONE', *, *, #2998, .F. ) ;
#762 = CARTESIAN_POINT ( 'NONE',  ( -7.450717329638298914, 23.86413627455948472, 32.76425935539839429 ) ) ;
#763 = DIRECTION ( 'NONE',  ( -1.000000000000000000, 0.000000000000000000, 0.000000000000000000 ) ) ;
#764 = LINE ( 'NONE', #3587, #1849 ) ;
#765 = DIRECTION ( 'NONE',  ( -1.000000000000000000, 0.000000000000000000, 0.000000000000000000 ) ) ;
#766 = ORIENTED_EDGE ( 'NONE', *, *, #3453, .F. ) ;
#767 = CARTESIAN_POINT ( 'NONE',  ( 197.0000000000000000, 68.99999999999997158, 110.0000000000000000 ) ) ;
#768 = VERTEX_POINT ( 'NONE', #2167 ) ;
#769 = DIRECTION ( 'NONE',  ( -1.000000000000000000, 0.000000000000000000, 0.000000000000000000 ) ) ;
#770 = DIRECTION ( 'NONE',  ( -0.000000000000000000, -0.000000000000000000, -1.000000000000000000 ) ) ;
#771 = ORIENTED_EDGE ( 'NONE', *, *, #5541, .T. ) ;
#772 = PRODUCT_DEFINITION_SHAPE ( 'NONE', 'NONE',  #6370 ) ;
#773 = ADVANCED_FACE ( 'NONE', ( #1755 ), #1233, .T. ) ;
#774 = CARTESIAN_POINT ( 'NONE',  ( 59.99991398172927859, 30.92345909152286154, 281.0000000000000000 ) ) ;
#775 = VERTEX_POINT ( 'NONE', #733 ) ;
#776 = EDGE_CURVE ( 'NONE', #3357, #6130, #2680, .T. ) ;
#777 = DIRECTION ( 'NONE',  ( -1.000000000000000000, 0.000000000000000000, 0.000000000000000000 ) ) ;
#778 = CARTESIAN_POINT ( 'NONE',  ( 2.380270672502711906E-15, -5.204170427930421283E-15, -195.0000000000000000 ) ) ;
#779 = DIRECTION ( 'NONE',  ( 0.000000000000000000, 0.000000000000000000, -1.000000000000000000 ) ) ;
#780 = ORIENTED_EDGE ( 'NONE', *, *, #1722, .T. ) ;
#781 = DIRECTION ( 'NONE',  ( 1.000000000000000000, 0.000000000000000000, 0.000000000000000000 ) ) ;
#782 = ORIENTED_EDGE ( 'NONE', *, *, #4549, .T. ) ;
#783 = CARTESIAN_POINT ( 'NONE',  ( 3.330617891528926844, 24.78132568362453370, 38.51271458136145753 ) ) ;
#784 = DIRECTION ( 'NONE',  ( -0.000000000000000000, -0.000000000000000000, -1.000000000000000000 ) ) ;
#785 = ADVANCED_FACE ( 'NONE', ( #6077, #2707 ), #2227, .T. ) ;
#786 = EDGE_CURVE ( 'NONE', #3016, #2696, #2527, .T. ) ;
#787 = CARTESIAN_POINT ( 'NONE',  ( 6.500000000000000000, 0.000000000000000000, 0.000000000000000000 ) ) ;
#788 = DIRECTION ( 'NONE',  ( -1.000000000000000000, 0.000000000000000000, 0.000000000000000000 ) ) ;
#789 = ORIENTED_EDGE ( 'NONE', *, *, #2310, .T. ) ;
#790 = ORIENTED_EDGE ( 'NONE', *, *, #6358, .T. ) ;
#791 = EDGE_CURVE ( 'NONE', #6038, #1386, #6343, .T. ) ;
#792 = CARTESIAN_POINT ( 'NONE',  ( -4.375754180095210444, 24.61494036324240398, 25.67889403490023881 ) ) ;
#793 = CARTESIAN_POINT ( 'NONE',  ( 17.00000000000000000, 2.081899558550500280E-15, 23.00000000000000000 ) ) ;
#794 = CARTESIAN_POINT ( 'NONE',  ( -15.99408614349810698, -19.21429697996681440, -4.336808689942017736E-15 ) ) ;
#795 = CYLINDRICAL_SURFACE ( 'NONE', #825, 90.00000000000000000 ) ;
#796 = ADVANCED_FACE ( 'NONE', ( #4678 ), #5202, .T. ) ;
#797 = AXIS2_PLACEMENT_3D ( 'NONE', #2741, #3618, #310 ) ;
#798 = ORIENTED_EDGE ( 'NONE', *, *, #363, .F. ) ;
#799 = CARTESIAN_POINT ( 'NONE',  ( -44.00000000000000000, -13.41640786499873350, -30.00000000000000000 ) ) ;
#800 = ORIENTED_EDGE ( 'NONE', *, *, #6223, .T. ) ;
#801 = EDGE_CURVE ( 'NONE', #713, #5661, #382, .T. ) ;
#802 = VECTOR ( 'NONE', #718, 1000.000000000000000 ) ;
#803 = DIRECTION ( 'NONE',  ( -1.000000000000000000, 0.000000000000000000, 0.000000000000000000 ) ) ;
#804 = CARTESIAN_POINT ( 'NONE',  ( -8.336125322366124024, -21.45114114349586387, 7.948328953041721157 ) ) ;
#805 = ORIENTED_EDGE ( 'NONE', *, *, #6094, .F. ) ;
#806 = CARTESIAN_POINT ( 'NONE',  ( -8.000000000000007105, 72.93807001241029297, 12.00000000000000000 ) ) ;
#807 = ORIENTED_EDGE ( 'NONE', *, *, #3257, .T. ) ;
#808 = DIRECTION ( 'NONE',  ( 0.000000000000000000, -0.000000000000000000, -1.000000000000000000 ) ) ;
#809 = FACE_OUTER_BOUND ( 'NONE', #513, .T. ) ;
#810 = CARTESIAN_POINT ( 'NONE',  ( 0.000000000000000000, 0.000000000000000000, -49.99999999999999289 ) ) ;
#811 = CIRCLE ( 'NONE', #4502, 89.87058297576894006 ) ;
#812 = CARTESIAN_POINT ( 'NONE',  ( -7.257437786822881876, -23.92362332953076276, 33.72945147699582691 ) ) ;
#813 = ORIENTED_EDGE ( 'NONE', *, *, #1612, .T. ) ;
#814 = SURFACE_SIDE_STYLE ('',( #905 ) ) ;
#815 = ORIENTED_EDGE ( 'NONE', *, *, #5748, .F. ) ;
#816 = CARTESIAN_POINT ( 'NONE',  ( 7.499981071996971949, 23.84848598800518715, 32.02274772221157662 ) ) ;
#817 = CARTESIAN_POINT ( 'NONE',  ( 4.061217559732478222, 22.64157742495655512, 38.09601054039983836 ) ) ;
#818 = CIRCLE ( 'NONE', #93, 23.00000000000000000 ) ;
#819 = DIRECTION ( 'NONE',  ( -1.000000000000000000, 1.224646799147352468E-16, 0.000000000000000000 ) ) ;
#820 = CARTESIAN_POINT ( 'NONE',  ( 3.336113272159680232, -24.78061407909199332, 25.03989924742863948 ) ) ;
#821 = ORIENTED_EDGE ( 'NONE', *, *, #4137, .F. ) ;
#822 = AXIS2_PLACEMENT_3D ( 'NONE', #4680, #2681, #1234 ) ;
#823 = VERTEX_POINT ( 'NONE', #4229 ) ;
#824 = CARTESIAN_POINT ( 'NONE',  ( -0.9883880857196325476, 24.98510658176930832, 24.32423833034778937 ) ) ;
#825 = AXIS2_PLACEMENT_3D ( 'NONE', #2264, #4127, #6205 ) ;
#826 = DIRECTION ( 'NONE',  ( 1.000000000000000000, 0.000000000000000000, 0.000000000000000000 ) ) ;
#827 = CARTESIAN_POINT ( 'NONE',  ( 0.000000000000000000, -25.00000000000000000, -20.00000000000000000 ) ) ;
#828 = DIRECTION ( 'NONE',  ( -1.000000000000000000, 0.000000000000000000, 0.000000000000000000 ) ) ;
#829 = VECTOR ( 'NONE', #2966, 1000.000000000000000 ) ;
#830 = ORIENTED_EDGE ( 'NONE', *, *, #483, .T. ) ;
#831 = EDGE_LOOP ( 'NONE', ( #233, #3348, #2987, #821 ) ) ;
#832 = ORIENTED_EDGE ( 'NONE', *, *, #6189, .T. ) ;
#833 = DIRECTION ( 'NONE',  ( 0.000000000000000000, -1.000000000000000000, -1.740526192617802767E-17 ) ) ;
#834 = AXIS2_PLACEMENT_3D ( 'NONE', #162, #1208, #5153 ) ;
#835 = CARTESIAN_POINT ( 'NONE',  ( 5.943311860187945328, -22.23481035324009270, 8.999810584836245297 ) ) ;
#836 = CARTESIAN_POINT ( 'NONE',  ( -15.99408614349810698, 19.21429697996681796, -4.336808689942017736E-15 ) ) ;
#837 = ORIENTED_EDGE ( 'NONE', *, *, #4553, .F. ) ;
#838 = CLOSED_SHELL ( 'NONE', ( #3926, #472, #2141, #4596, #6202, #3144, #3539, #5587, #5826, #2784, #995, #5539, #2322, #208, #1807, #4835 ) ) ;
#839 = CARTESIAN_POINT ( 'NONE',  ( 0.000000000000000000, 0.000000000000000000, -240.0000000000000000 ) ) ;
#840 = ORIENTED_EDGE ( 'NONE', *, *, #305, .F. ) ;
#841 = DIRECTION ( 'NONE',  ( -0.000000000000000000, -0.000000000000000000, 1.000000000000000000 ) ) ;
#842 = CIRCLE ( 'NONE', #1437, 90.00000000000000000 ) ;
#843 = CARTESIAN_POINT ( 'NONE',  ( 19.25293315802950644, 8.385974291186926166, 0.000000000000000000 ) ) ;
#844 = CARTESIAN_POINT ( 'NONE',  ( 237.0000000000000284, 68.99999999999997158, 110.0000000000000000 ) ) ;
#845 = CARTESIAN_POINT ( 'NONE',  ( -5.649026277996909151, -24.35594688685564790, 26.81770774654597744 ) ) ;
#846 = ORIENTED_EDGE ( 'NONE', *, *, #3676, .F. ) ;
#847 = DIRECTION ( 'NONE',  ( -0.000000000000000000, -0.000000000000000000, 1.000000000000000000 ) ) ;
#848 = EDGE_LOOP ( 'NONE', ( #6233, #2139, #3706, #4614 ) ) ;
#849 = AXIS2_PLACEMENT_3D ( 'NONE', #4076, #1637, #5460 ) ;
#850 = CARTESIAN_POINT ( 'NONE',  ( -7.182657412981705209E-17, 20.00000000000000711, 39.27501000028011902 ) ) ;
#851 = DIRECTION ( 'NONE',  ( -0.000000000000000000, -0.000000000000000000, -1.000000000000000000 ) ) ;
#852 = DIRECTION ( 'NONE',  ( 0.000000000000000000, 0.000000000000000000, -1.000000000000000000 ) ) ;
#853 = CARTESIAN_POINT ( 'NONE',  ( 2.223777455422794702, -22.89327810718596368, 24.60873847605252251 ) ) ;
#854 = ORIENTED_EDGE ( 'NONE', *, *, #1411, .T. ) ;
#855 = ORIENTED_EDGE ( 'NONE', *, *, #6026, .F. ) ;
#856 = CARTESIAN_POINT ( 'NONE',  ( -21.00000000000000355, 0.000000000000000000, 12.00000000000000000 ) ) ;
#857 = DIRECTION ( 'NONE',  ( 0.000000000000000000, 0.000000000000000000, -1.000000000000000000 ) ) ;
#858 = DIRECTION ( 'NONE',  ( 1.000000000000000000, 0.000000000000000000, 0.000000000000000000 ) ) ;
#859 = CARTESIAN_POINT ( 'NONE',  ( 0.000000000000000000, 0.000000000000000000, 51.00000000000002842 ) ) ;
#860 = EDGE_CURVE ( 'NONE', #590, #5090, #4386, .T. ) ;
#861 = VERTEX_POINT ( 'NONE', #1656 ) ;
#862 = VERTEX_POINT ( 'NONE', #701 ) ;
#863 = ORIENTED_EDGE ( 'NONE', *, *, #1531, .F. ) ;
#864 = VECTOR ( 'NONE', #784, 1000.000000000000000 ) ;
#865 = EDGE_CURVE ( 'NONE', #1470, #4878, #3658, .T. ) ;
#866 = LINE ( 'NONE', #4785, #2269 ) ;
#867 = APPLICATION_CONTEXT ( 'automotive_design' ) ;
#868 = ITEM_DEFINED_TRANSFORMATION ( 'NONE', 'NONE', #5222,  #6349 ) ;
#869 = DIRECTION ( 'NONE',  ( 0.000000000000000000, -1.000000000000000000, 0.000000000000000000 ) ) ;
#870 = FACE_OUTER_BOUND ( 'NONE', #2801, .T. ) ;
#871 = EDGE_LOOP ( 'NONE', ( #4711, #3275, #3161, #6176 ) ) ;
#872 = EDGE_LOOP ( 'NONE', ( #950, #2470, #2429, #6101 ) ) ;
#873 = CARTESIAN_POINT ( 'NONE',  ( -6.500000000000000000, 8.572527594031472204E-16, 0.000000000000000000 ) ) ;
#874 = DIRECTION ( 'NONE',  ( 1.000000000000000000, 0.000000000000000000, 0.000000000000000000 ) ) ;
#875 = EDGE_CURVE ( 'NONE', #306, #2898, #5816, .T. ) ;
#876 = CARTESIAN_POINT ( 'NONE',  ( 6.500000000000000000, 0.000000000000000000, 12.00000000000000000 ) ) ;
#877 = CARTESIAN_POINT ( 'NONE',  ( -7.499981071996971949, -23.84848598800519426, 32.02274772221159083 ) ) ;
#878 = ORIENTED_EDGE ( 'NONE', *, *, #5629, .F. ) ;
#879 = DIRECTION ( 'NONE',  ( 1.000000000000000000, 0.000000000000000000, 0.000000000000000000 ) ) ;
#880 = DIRECTION ( 'NONE',  ( 0.000000000000000000, 0.000000000000000000, 1.000000000000000000 ) ) ;
#881 = PLANE ( 'NONE',  #4790 ) ;
#882 = CARTESIAN_POINT ( 'NONE',  ( -13.14183123006980480, 39.58265509608657595, -180.0000000000000000 ) ) ;
#883 = CARTESIAN_POINT ( 'NONE',  ( 0.4986381067920973575, -25.00000000000001421, 24.27501000028011191 ) ) ;
#884 = ORIENTED_EDGE ( 'NONE', *, *, #4544, .F. ) ;
#885 = ORIENTED_EDGE ( 'NONE', *, *, #305, .T. ) ;
#886 = CARTESIAN_POINT ( 'NONE',  ( -1.957817464472356495, 24.92794428843967580, 39.03180047523679974 ) ) ;
#887 = DIRECTION ( 'NONE',  ( -0.000000000000000000, -0.000000000000000000, 1.000000000000000000 ) ) ;
#888 = DIRECTION ( 'NONE',  ( 1.000000000000000000, 0.000000000000000000, 0.000000000000000000 ) ) ;
#889 = PLANE ( 'NONE',  #1635 ) ;
#890 = ORIENTED_EDGE ( 'NONE', *, *, #2776, .T. ) ;
#891 = ORIENTED_EDGE ( 'NONE', *, *, #2377, .F. ) ;
#892 = CARTESIAN_POINT ( 'NONE',  ( 132.0000000000000000, 69.00000000000000000, 110.0000000000000000 ) ) ;
#894 = VECTOR ( 'NONE', #3755, 1000.000000000000000 ) ;
#893 = ITEM_DEFINED_TRANSFORMATION ( 'NONE', 'NONE', #1306,  #6349 ) ;
#895 = FACE_OUTER_BOUND ( 'NONE', #119, .T. ) ;
#896 = CIRCLE ( 'NONE', #1523, 21.00000000000000355 ) ;
#897 = CYLINDRICAL_SURFACE ( 'NONE', #2061, 22.00000000000000000 ) ;
#898 = ORIENTED_EDGE ( 'NONE', *, *, #776, .F. ) ;
#899 = DIRECTION ( 'NONE',  ( 0.000000000000000000, 0.000000000000000000, -1.000000000000000000 ) ) ;
#900 = AXIS2_PLACEMENT_3D ( 'NONE', #3588, #2957, #4370 ) ;
#901 = CARTESIAN_POINT ( 'NONE',  ( -5.103812965180195782, -22.42723062334006556, 26.27493091522155666 ) ) ;
#902 = DIRECTION ( 'NONE',  ( 0.000000000000000000, 1.000000000000000000, 1.239088197126290570E-16 ) ) ;
#903 = CARTESIAN_POINT ( 'NONE',  ( -7.019376005445151279, -23.99453911528665984, 29.12205218481383540 ) ) ;
#904 = ORIENTED_EDGE ( 'NONE', *, *, #4382, .F. ) ;
#905 = SURFACE_STYLE_FILL_AREA ( #5807 ) ;
#906 = AXIS2_PLACEMENT_3D ( 'NONE', #1949, #2549, #985 ) ;
#907 = CARTESIAN_POINT ( 'NONE',  ( -3.061616997868383043E-15, -25.00000000000000000, -130.0000000000000000 ) ) ;
#908 = CIRCLE ( 'NONE', #5628, 21.00000000000000355 ) ;
#909 = DIRECTION ( 'NONE',  ( 0.000000000000000000, 0.000000000000000000, 1.000000000000000000 ) ) ;
#910 = CARTESIAN_POINT ( 'NONE',  ( 6.801000575755121069, -21.97168837322005075, 28.60528907419297084 ) ) ;
#911 = ORIENTED_EDGE ( 'NONE', *, *, #3393, .F. ) ;
#912 = CARTESIAN_POINT ( 'NONE',  ( 8.000000000000007105, 72.93807001241029297, 12.00000000000000000 ) ) ;
#913 = AXIS2_PLACEMENT_3D ( 'NONE', #4319, #5208, #2232 ) ;
#914 = ORIENTED_EDGE ( 'NONE', *, *, #5064, .F. ) ;
#915 = CARTESIAN_POINT ( 'NONE',  ( -3.471216600621237713, 22.73745234227088829, 38.42710443719838054 ) ) ;
#916 = AXIS2_PLACEMENT_3D ( 'NONE', #351, #3139, #6242 ) ;
#917 = CARTESIAN_POINT ( 'NONE',  ( -44.43364355155666345, 29.42304313293565343, -49.99999999999999289 ) ) ;
#918 = CARTESIAN_POINT ( 'NONE',  ( 0.000000000000000000, 0.000000000000000000, -115.0000000000000000 ) ) ;
#919 = VECTOR ( 'NONE', #5261, 1000.000000000000000 ) ;
#920 = CARTESIAN_POINT ( 'NONE',  ( 0.000000000000000000, 0.000000000000000000, -175.0000000000000284 ) ) ;
#921 = ORIENTED_EDGE ( 'NONE', *, *, #3930, .F. ) ;
#922 = ORIENTED_EDGE ( 'NONE', *, *, #1260, .F. ) ;
#923 = ORIENTED_EDGE ( 'NONE', *, *, #3930, .T. ) ;
#924 = AXIS2_PLACEMENT_3D ( 'NONE', #2743, #4649, #5658 ) ;
#925 = CIRCLE ( 'NONE', #4616, 21.00000000000000355 ) ;
#926 = CARTESIAN_POINT ( 'NONE',  ( -0.2052511266214760433, -21.25619793154163517, -160.0000000000000284 ) ) ;
#927 = CARTESIAN_POINT ( 'NONE',  ( -13.27340567884428957, 26.93747317953756593, 8.027960515371221462 ) ) ;
#928 = DIRECTION ( 'NONE',  ( -0.000000000000000000, -0.000000000000000000, 1.000000000000000000 ) ) ;
#929 = ORIENTED_EDGE ( 'NONE', *, *, #2377, .T. ) ;
#930 = ITEM_DEFINED_TRANSFORMATION ( 'NONE', 'NONE', #5743,  #6349 ) ;
#931 = VECTOR ( 'NONE', #1379, 1000.000000000000000 ) ;
#932 = CARTESIAN_POINT ( 'NONE',  ( 0.000000000000000000, 0.000000000000000000, -180.0000000000000000 ) ) ;
#933 = DIRECTION ( 'NONE',  ( 1.000000000000000000, 0.000000000000000000, 0.000000000000000000 ) ) ;
#934 = DIRECTION ( 'NONE',  ( 0.000000000000000000, -1.000000000000000000, 0.000000000000000000 ) ) ;
#935 = CARTESIAN_POINT ( 'NONE',  ( 67.00000000000000000, 69.00000000000000000, 110.0000000000000000 ) ) ;
#936 = CARTESIAN_POINT ( 'NONE',  ( 44.43364355155687662, -29.42304313293534790, -195.0000000000000000 ) ) ;
#937 = ORIENTED_EDGE ( 'NONE', *, *, #5904, .T. ) ;
#938 = EDGE_CURVE ( 'NONE', #5509, #2206, #3462, .T. ) ;
#939 = PRESENTATION_STYLE_ASSIGNMENT (( #3251 ) ) ;
#940 = ADVANCED_FACE ( 'NONE', ( #3908 ), #2902, .F. ) ;
#941 = COLOUR_RGB ( '',0.7921568627450980005, 0.8196078431372548767, 0.9333333333333333481 ) ;
#942 = VECTOR ( 'NONE', #515, 1000.000000000000000 ) ;
#943 = DIRECTION ( 'NONE',  ( -0.000000000000000000, -0.000000000000000000, -1.000000000000000000 ) ) ;
#944 = EDGE_CURVE ( 'NONE', #2247, #635, #2364, .T. ) ;
#945 = FACE_OUTER_BOUND ( 'NONE', #2573, .T. ) ;
#946 = EDGE_CURVE ( 'NONE', #3551, #4017, #5790, .T. ) ;
#947 = EDGE_CURVE ( 'NONE', #3745, #4120, #66, .T. ) ;
#948 = DIRECTION ( 'NONE',  ( 0.000000000000000000, 0.000000000000000000, 1.000000000000000000 ) ) ;
#949 = CARTESIAN_POINT ( 'NONE',  ( 4.240260142090316542, -22.60916465144881826, 25.57229111368760854 ) ) ;
#950 = ORIENTED_EDGE ( 'NONE', *, *, #464, .F. ) ;
#951 = DIRECTION ( 'NONE',  ( -1.000000000000000000, 0.000000000000000000, 0.000000000000000000 ) ) ;
#952 = DIRECTION ( 'NONE',  ( 1.000000000000000000, 0.000000000000000000, 0.000000000000000000 ) ) ;
#953 = CARTESIAN_POINT ( 'NONE',  ( -6.980300741495532257, 21.91538084489497962, 34.52732716285097325 ) ) ;
#954 = AXIS2_PLACEMENT_3D ( 'NONE', #5775, #5188, #1351 ) ;
#955 = PLANE ( 'NONE',  #2021 ) ;
#956 = DIRECTION ( 'NONE',  ( 1.000000000000000000, 0.000000000000000000, 0.000000000000000000 ) ) ;
#957 = DIRECTION ( 'NONE',  ( 0.000000000000000000, -0.000000000000000000, 1.000000000000000000 ) ) ;
#958 = ORIENTED_EDGE ( 'NONE', *, *, #1201, .F. ) ;
#959 = VERTEX_POINT ( 'NONE', #5334 ) ;
#960 = ORIENTED_EDGE ( 'NONE', *, *, #5044, .T. ) ;
#961 = LINE ( 'NONE', #4434, #942 ) ;
#962 = DIRECTION ( 'NONE',  ( -0.000000000000000000, -0.000000000000000000, -1.000000000000000000 ) ) ;
#963 = AXIS2_PLACEMENT_3D ( 'NONE', #3288, #3710, #5266 ) ;
#964 = CARTESIAN_POINT ( 'NONE',  ( 10.34785354329971341, -22.76990768458740533, 6.703770685560596299 ) ) ;
#965 = ORIENTED_EDGE ( 'NONE', *, *, #4589, .T. ) ;
#966 = DIRECTION ( 'NONE',  ( 0.000000000000000000, -0.000000000000000000, -1.000000000000000000 ) ) ;
#967 = CARTESIAN_POINT ( 'NONE',  ( -7.210417624014669791, -21.84081640740546248, 33.88833234030835229 ) ) ;
#968 = EDGE_CURVE ( 'NONE', #1691, #1557, #2295, .T. ) ;
#969 = LINE ( 'NONE', #2080, #5844 ) ;
#970 = FACE_OUTER_BOUND ( 'NONE', #3101, .T. ) ;
#971 = ORIENTED_EDGE ( 'NONE', *, *, #2591, .F. ) ;
#972 = CARTESIAN_POINT ( 'NONE',  ( 4.592425496802570422E-15, 25.00000000000000000, 0.000000000000000000 ) ) ;
#973 = CARTESIAN_POINT ( 'NONE',  ( -8.000000000000007105, 72.93807001241029297, 9.999999999999996447 ) ) ;
#974 = EDGE_CURVE ( 'NONE', #3152, #2130, #3352, .T. ) ;
#975 = CARTESIAN_POINT ( 'NONE',  ( -13.30660938351090117, 26.80958678890347358, 4.207676383415306809 ) ) ;
#976 = ORIENTED_EDGE ( 'NONE', *, *, #1918, .F. ) ;
#977 = DIRECTION ( 'NONE',  ( 0.000000000000000000, -0.000000000000000000, 1.000000000000000000 ) ) ;
#978 = ORIENTED_EDGE ( 'NONE', *, *, #3238, .T. ) ;
#979 = CARTESIAN_POINT ( 'NONE',  ( 7.200995294576264527, 21.84734027758491237, 8.482870732638906119 ) ) ;
#980 = EDGE_CURVE ( 'NONE', #1773, #3440, #1187, .T. ) ;
#981 = VERTEX_POINT ( 'NONE', #6328 ) ;
#982 = DIRECTION ( 'NONE',  ( 1.000000000000000000, 0.000000000000000000, 0.000000000000000000 ) ) ;
#983 = ADVANCED_FACE ( 'NONE', ( #5851, #5886 ), #955, .T. ) ;
#984 = PLANE ( 'NONE',  #1975 ) ;
#985 = DIRECTION ( 'NONE',  ( 1.836970198721029194E-16, 1.000000000000000000, 0.000000000000000000 ) ) ;
#986 = CARTESIAN_POINT ( 'NONE',  ( 44.64065620456912598, 28.99954194078667413, -115.0000000000000000 ) ) ;
#987 = ORIENTED_EDGE ( 'NONE', *, *, #2859, .F. ) ;
#988 = EDGE_CURVE ( 'NONE', #2898, #2909, #4798, .T. ) ;
#989 = EDGE_LOOP ( 'NONE', ( #5388, #3169 ) ) ;
#990 = VERTEX_POINT ( 'NONE', #5758 ) ;
#991 = CARTESIAN_POINT ( 'NONE',  ( 0.000000000000000000, 0.000000000000000000, 110.0000000000000000 ) ) ;
#992 = CIRCLE ( 'NONE', #5075, 90.00000000000321165 ) ;
#993 = DIRECTION ( 'NONE',  ( -0.000000000000000000, -0.000000000000000000, -1.000000000000000000 ) ) ;
#994 = VECTOR ( 'NONE', #1447, 1000.000000000000000 ) ;
#995 = ADVANCED_FACE ( 'NONE', ( #465 ), #2424, .F. ) ;
#996 = CARTESIAN_POINT ( 'NONE',  ( 15.99408614349810698, -19.21429697996681440, 0.000000000000000000 ) ) ;
#997 = VERTEX_POINT ( 'NONE', #3816 ) ;
#998 = CARTESIAN_POINT ( 'NONE',  ( -44.64065620456596406, -28.99954194078535963, 15.00000000000000000 ) ) ;
#999 = CARTESIAN_POINT ( 'NONE',  ( -0.2247101425308446754, -23.00000000000000355, 24.27501000028010480 ) ) ;
#1000 = FACE_OUTER_BOUND ( 'NONE', #6254, .T. ) ;
#1001 = LINE ( 'NONE', #489, #2259 ) ;
#1002 = ORIENTED_EDGE ( 'NONE', *, *, #28, .T. ) ;
#1003 = DIRECTION ( 'NONE',  ( -0.000000000000000000, -0.000000000000000000, -1.000000000000000000 ) ) ;
#1004 = CARTESIAN_POINT ( 'NONE',  ( 17.00000000000000000, 0.000000000000000000, -115.0000000000000000 ) ) ;
#1005 = CARTESIAN_POINT ( 'NONE',  ( 0.000000000000000000, 0.000000000000000000, 47.00000000000000711 ) ) ;
#1006 = CARTESIAN_POINT ( 'NONE',  ( -17.00000000000000000, 2.081899558550500280E-15, -115.0000000000000000 ) ) ;
#1007 = CARTESIAN_POINT ( 'NONE',  ( 9.184177739184520255E-16, -25.00000000000000000, 39.27501000028010480 ) ) ;
#1008 = VERTEX_POINT ( 'NONE', #1821 ) ;
#1009 = SURFACE_SIDE_STYLE ('',( #1462 ) ) ;
#1010 = CARTESIAN_POINT ( 'NONE',  ( 13.41482486054666445, 26.39531364385071655, 6.264720534548224862 ) ) ;
#1011 = CARTESIAN_POINT ( 'NONE',  ( 0.000000000000000000, 0.000000000000000000, 16.00000000000000000 ) ) ;
#1012 = AXIS2_PLACEMENT_3D ( 'NONE', #3258, #368, #2323 ) ;
#1013 = CARTESIAN_POINT ( 'NONE',  ( 64.99991398172927859, 76.99999716619419132, 281.0000000000000000 ) ) ;
#1014 = CARTESIAN_POINT ( 'NONE',  ( 22.21770253897382474, 3.871672004622519037, -95.00000000000000000 ) ) ;
#1015 = DIRECTION ( 'NONE',  ( -1.000000000000000000, 0.000000000000000000, 0.000000000000000000 ) ) ;
#1016 = ORIENTED_EDGE ( 'NONE', *, *, #2472, .T. ) ;
#1017 = AXIS2_PLACEMENT_3D ( 'NONE', #2237, #5695, #1277 ) ;
#1018 = ORIENTED_EDGE ( 'NONE', *, *, #4355, .F. ) ;
#1019 = VERTEX_POINT ( 'NONE', #1466 ) ;
#1020 = VERTEX_POINT ( 'NONE', #4387 ) ;
#1021 = FACE_OUTER_BOUND ( 'NONE', #3299, .T. ) ;
#1022 = DIRECTION ( 'NONE',  ( 1.000000000000000000, 0.000000000000000000, 0.000000000000000000 ) ) ;
#1023 = CARTESIAN_POINT ( 'NONE',  ( 3.487686359055458762, -24.77054744280749432, 9.676329747922178370 ) ) ;
#1024 = ORIENTED_EDGE ( 'NONE', *, *, #395, .T. ) ;
#1025 = CIRCLE ( 'NONE', #5353, 7.500000000000000000 ) ;
#1026 = VECTOR ( 'NONE', #508, 1000.000000000000000 ) ;
#1027 = SHAPE_DEFINITION_REPRESENTATION ( #5088, #5606 ) ;
#1028 = DIRECTION ( 'NONE',  ( 1.000000000000000000, 0.000000000000000000, 0.000000000000000000 ) ) ;
#1029 = FACE_OUTER_BOUND ( 'NONE', #5572, .T. ) ;
#1030 = VERTEX_POINT ( 'NONE', #6356 ) ;
#1031 = DIRECTION ( 'NONE',  ( -1.000000000000000000, 0.000000000000000000, 0.000000000000000000 ) ) ;
#1032 = DIRECTION ( 'NONE',  ( -1.000000000000000000, 0.000000000000000000, 0.000000000000000000 ) ) ;
#1033 = CARTESIAN_POINT ( 'NONE',  ( 2.546401178541497462E-16, 25.00000000000000000, 24.27501000028010125 ) ) ;
#1034 = CIRCLE ( 'NONE', #5562, 25.00000000000000000 ) ;
#1035 = CARTESIAN_POINT ( 'NONE',  ( -1.239954884136695111E-14, -67.50000000000000000, 276.0000000000000000 ) ) ;
#1036 = CARTESIAN_POINT ( 'NONE',  ( -43.99999999999987921, 13.41640786499904969, -110.0000000000000000 ) ) ;
#1037 = ORIENTED_EDGE ( 'NONE', *, *, #5028, .T. ) ;
#1038 = AXIS2_PLACEMENT_3D ( 'NONE', #6110, #1720, #769 ) ;
#1039 = ORIENTED_EDGE ( 'NONE', *, *, #2197, .F. ) ;
#1040 = CARTESIAN_POINT ( 'NONE',  ( -5.576854706809766249, 22.31420130230918986, 36.79476692679597249 ) ) ;
#1041 = DIRECTION ( 'NONE',  ( -0.000000000000000000, 1.000000000000000000, -0.000000000000000000 ) ) ;
#1042 = LINE ( 'NONE', #112, #2539 ) ;
#1043 = FACE_OUTER_BOUND ( 'NONE', #5070, .T. ) ;
#1044 = VERTEX_POINT ( 'NONE', #3421 ) ;
#1045 = EDGE_LOOP ( 'NONE', ( #2012, #5927, #2089, #1195 ) ) ;
#1046 = VECTOR ( 'NONE', #1041, 1000.000000000000000 ) ;
#1047 = LINE ( 'NONE', #1620, #6135 ) ;
#1048 = EDGE_CURVE ( 'NONE', #4162, #3651, #2774, .T. ) ;
#1049 = CARTESIAN_POINT ( 'NONE',  ( 0.2052511266213299934, 21.25619793154162807, -180.0000000000000000 ) ) ;
#1050 = PLANE ( 'NONE',  #1622 ) ;
#1051 = ORIENTED_EDGE ( 'NONE', *, *, #2508, .F. ) ;
#1052 = EDGE_CURVE ( 'NONE', #635, #5193, #6086, .T. ) ;
#1053 = DIRECTION ( 'NONE',  ( 4.267800137145458322E-16, 0.000000000000000000, 1.000000000000000000 ) ) ;
#1054 = LINE ( 'NONE', #5595, #4990 ) ;
#1055 = DIRECTION ( 'NONE',  ( 1.000000000000000000, 1.852483853906148040E-16, -0.000000000000000000 ) ) ;
#1056 = EDGE_LOOP ( 'NONE', ( #5923, #2799, #5555, #2712 ) ) ;
#1057 = DIRECTION ( 'NONE',  ( 1.000000000000000000, 0.000000000000000000, -0.000000000000000000 ) ) ;
#1058 = EDGE_CURVE ( 'NONE', #602, #51, #1886, .T. ) ;
#1059 = DIRECTION ( 'NONE',  ( 0.000000000000000000, 0.000000000000000000, 1.000000000000000000 ) ) ;
#1060 = EDGE_CURVE ( 'NONE', #5377, #633, #3845, .T. ) ;
#1061 = DIRECTION ( 'NONE',  ( -0.000000000000000000, -0.000000000000000000, -1.000000000000000000 ) ) ;
#1062 = CARTESIAN_POINT ( 'NONE',  ( -44.43364355155666345, 29.42304313293564988, -115.0000000000000000 ) ) ;
#1063 = EDGE_LOOP ( 'NONE', ( #4947, #720 ) ) ;
#1064 = ADVANCED_FACE ( 'NONE', ( #1149 ), #3631, .F. ) ;
#1065 =( NAMED_UNIT ( * ) SI_UNIT ( $, .STERADIAN. ) SOLID_ANGLE_UNIT ( ) );
#1066 = DIRECTION ( 'NONE',  ( 1.000000000000000000, 0.000000000000000000, 0.000000000000000000 ) ) ;
#1067 = CARTESIAN_POINT ( 'NONE',  ( 6.383431969492757929, 22.09754339782970334, 27.81230622618427617 ) ) ;
#1068 = FACE_OUTER_BOUND ( 'NONE', #871, .T. ) ;
#1069 = CARTESIAN_POINT ( 'NONE',  ( 7.947562104483774093, 68.75545066608756883, 0.000000000000000000 ) ) ;
#1070 = VERTEX_POINT ( 'NONE', #2179 ) ;
#1071 = VERTEX_POINT ( 'NONE', #5602 ) ;
#1072 = ORIENTED_EDGE ( 'NONE', *, *, #980, .T. ) ;
#1073 = DIRECTION ( 'NONE',  ( 0.000000000000000000, 1.000000000000000000, 0.000000000000000000 ) ) ;
#1074 = PLANE ( 'NONE',  #3046 ) ;
#1075 = DIRECTION ( 'NONE',  ( -0.000000000000000000, -0.000000000000000000, -1.000000000000000000 ) ) ;
#1076 = CARTESIAN_POINT ( 'NONE',  ( -12.19460461707455678, -21.82662405552711959, 5.169298567843259917 ) ) ;
#1077 = VERTEX_POINT ( 'NONE', #4942 ) ;
#1078 = AXIS2_PLACEMENT_3D ( 'NONE', #6011, #4579, #3617 ) ;
#1079 = SHAPE_DEFINITION_REPRESENTATION ( #3636, #1490 ) ;
#1080 = CARTESIAN_POINT ( 'NONE',  ( -4.061217559732478222, -22.64157742495655512, 38.09601054039983836 ) ) ;
#1081 = DIRECTION ( 'NONE',  ( 0.000000000000000000, -1.000000000000000000, 0.000000000000000000 ) ) ;
#1082 = EDGE_LOOP ( 'NONE', ( #1739, #987 ) ) ;
#1083 = CARTESIAN_POINT ( 'NONE',  ( 44.00000000000009948, 13.41640786499835514, -95.00000000000000000 ) ) ;
#1084 = AXIS2_PLACEMENT_3D ( 'NONE', #242, #181, #1197 ) ;
#1085 = CARTESIAN_POINT ( 'NONE',  ( 0.000000000000000000, 0.000000000000000000, 23.00000000000000000 ) ) ;
#1086 = DIRECTION ( 'NONE',  ( -0.000000000000000000, -0.000000000000000000, 1.000000000000000000 ) ) ;
#1087 = ORIENTED_EDGE ( 'NONE', *, *, #1531, .T. ) ;
#1088 = CIRCLE ( 'NONE', #2849, 89.87058297576894006 ) ;
#1089 = FACE_OUTER_BOUND ( 'NONE', #2840, .T. ) ;
#1090 = CARTESIAN_POINT ( 'NONE',  ( -15.82602517378898987, 37.28747423195201094, -225.0000000000000000 ) ) ;
#1091 = CARTESIAN_POINT ( 'NONE',  ( 5.722301980643075048, 22.27724803853372393, 26.92170784547232998 ) ) ;
#1092 = CARTESIAN_POINT ( 'NONE',  ( -12.21008954351328057, 21.81796696573388772, 5.154724438801039810 ) ) ;
#1093 = DIRECTION ( 'NONE',  ( 1.000000000000000000, 0.000000000000000000, 0.000000000000000000 ) ) ;
#1094 = ORIENTED_EDGE ( 'NONE', *, *, #2856, .F. ) ;
#1095 = EDGE_LOOP ( 'NONE', ( #6109, #1616, #3312, #3605, #890, #5404, #5243 ) ) ;
#1096 = ORIENTED_EDGE ( 'NONE', *, *, #1395, .T. ) ;
#1097 = AXIS2_PLACEMENT_3D ( 'NONE', #2904, #3422, #5977 ) ;
#1098 = DIRECTION ( 'NONE',  ( -1.000000000000000000, 0.000000000000000000, 0.000000000000000000 ) ) ;
#1099 = DIRECTION ( 'NONE',  ( 1.000000000000000000, 0.000000000000000000, 0.000000000000000000 ) ) ;
#1100 = CARTESIAN_POINT ( 'NONE',  ( 44.00000000000009948, 13.41640786499835514, -115.0000000000000000 ) ) ;
#1101 = VECTOR ( 'NONE', #3349, 1000.000000000000000 ) ;
#1102 = FACE_OUTER_BOUND ( 'NONE', #5593, .T. ) ;
#1103 = FACE_OUTER_BOUND ( 'NONE', #1354, .T. ) ;
#1104 = ORIENTED_EDGE ( 'NONE', *, *, #664, .F. ) ;
#1105 = AXIS2_PLACEMENT_3D ( 'NONE', #1219, #259, #781 ) ;
#1106 = DIRECTION ( 'NONE',  ( 1.000000000000000000, 0.000000000000000000, 0.000000000000000000 ) ) ;
#1107 = ORIENTED_EDGE ( 'NONE', *, *, #5044, .F. ) ;
#1108 = VECTOR ( 'NONE', #418, 1000.000000000000000 ) ;
#1109 = CARTESIAN_POINT ( 'NONE',  ( 2.012341796004660122, -22.91179784512888773, 39.00000000000001421 ) ) ;
#1110 = ORIENTED_EDGE ( 'NONE', *, *, #5505, .F. ) ;
#1111 = B_SPLINE_CURVE_WITH_KNOTS ( 'NONE', 3,
 ( #3716, #728, #6127, #211, #6071, #3674, #5583, #5680, #266, #5101, #6098, #2162, #4119, #2222, #3641, #5648, #1227, #3192, #5171, #759, #4183, #6159, #1815, #5845, #5328, #340, #5752, #910, #6232, #5785, #1361, #1779, #3840, #2862, #949, #5810, #5713, #2806, #853, #2255, #1423, #4840, #5231, #431 ),
 .UNSPECIFIED., .F., .F.,
 ( 4, 2, 2, 2, 2, 2, 2, 2, 2, 2, 2, 2, 2, 2, 2, 2, 2, 2, 2, 2, 2, 4 ),
 ( 0.000000000000000000, 0.001348713335717714561, 0.002023070003576572708, 0.002697426671435430422, 0.004046140007153132406, 0.004720496675011990988, 0.005394853342870850436, 0.006743566678588568467, 0.007417923346447437456, 0.008092280014306306446, 0.009440993350024065242, 0.01078970668574182230, 0.01213842002145957069, 0.01281277668931844402, 0.01348713335717731908, 0.01483584669289507441, 0.01618456002861283147, 0.01753327336433058506, 0.01888198670004834212, 0.01955634336790721892, 0.02023070003576609918, 0.02157941337148385624 ),
 .UNSPECIFIED. ) ;
#1112 = AXIS2_PLACEMENT_3D ( 'NONE', #3105, #5591, #1757 ) ;
#1113 = CARTESIAN_POINT ( 'NONE',  ( -16.00000000000000000, 0.000000000000000000, 12.00000000000000000 ) ) ;
#1114 = VECTOR ( 'NONE', #218, 1000.000000000000000 ) ;
#1115 = CIRCLE ( 'NONE', #1850, 17.00000000000000000 ) ;
#1116 = ADVANCED_FACE ( 'NONE', ( #1181 ), #984, .T. ) ;
#1117 = LINE ( 'NONE', #2181, #4695 ) ;
#1118 = EDGE_CURVE ( 'NONE', #6264, #6324, #2972, .T. ) ;
#1119 = DIRECTION ( 'NONE',  ( -0.000000000000000000, -0.000000000000000000, 1.000000000000000000 ) ) ;
#1120 = ORIENTED_EDGE ( 'NONE', *, *, #4636, .F. ) ;
#1121 = CARTESIAN_POINT ( 'NONE',  ( -3.443445423526525051, 22.74486015987870147, 9.669004251864722121 ) ) ;
#1122 = EDGE_CURVE ( 'NONE', #117, #5057, #4136, .T. ) ;
#1123 = CYLINDRICAL_SURFACE ( 'NONE', #1649, 21.00000000000000355 ) ;
#1124 = CARTESIAN_POINT ( 'NONE',  ( 7.210417624014669791, 21.84081640740546248, 33.88833234030835229 ) ) ;
#1125 = VECTOR ( 'NONE', #5931, 1000.000000000000000 ) ;
#1126 = EDGE_CURVE ( 'NONE', #3949, #3812, #745, .T. ) ;
#1127 = ADVANCED_FACE ( 'NONE', ( #4972, #2492 ), #2604, .T. ) ;
#1128 = DIRECTION ( 'NONE',  ( 0.000000000000000000, -0.000000000000000000, -1.000000000000000000 ) ) ;
#1129 = CARTESIAN_POINT ( 'NONE',  ( -6.500000000000001776, 120.0000000000000000, 12.00000000000000000 ) ) ;
#1130 = ORIENTED_EDGE ( 'NONE', *, *, #517, .F. ) ;
#1131 = EDGE_LOOP ( 'NONE', ( #2914, #3327, #1369, #3217 ) ) ;
#1132 = ORIENTED_EDGE ( 'NONE', *, *, #4544, .T. ) ;
#1133 = FACE_BOUND ( 'NONE', #3515, .T. ) ;
#1134 = PRESENTATION_LAYER_ASSIGNMENT (  '', '', ( #1761 ) ) ;
#1135 = AXIS2_PLACEMENT_3D ( 'NONE', #3429, #5308, #2337 ) ;
#1136 = CYLINDRICAL_SURFACE ( 'NONE', #1240, 90.00000000000319744 ) ;
#1137 = ADVANCED_FACE ( 'NONE', ( #165 ), #539, .T. ) ;
#1138 = FACE_OUTER_BOUND ( 'NONE', #1617, .T. ) ;
#1139 = CARTESIAN_POINT ( 'NONE',  ( 0.000000000000000000, 0.000000000000000000, 0.000000000000000000 ) ) ;
#1140 = CARTESIAN_POINT ( 'NONE',  ( -15.63352991451900564, -19.51442596162454990, 0.7402269581920462027 ) ) ;
#1141 = ORIENTED_EDGE ( 'NONE', *, *, #5072, .T. ) ;
#1142 = CYLINDRICAL_SURFACE ( 'NONE', #15, 46.00000000000000000 ) ;
#1143 = LINE ( 'NONE', #5114, #1391 ) ;
#1144 = VERTEX_POINT ( 'NONE', #6088 ) ;
#1145 = CARTESIAN_POINT ( 'NONE',  ( 0.000000000000000000, -25.00000000000000000, -20.00000000000000000 ) ) ;
#1146 = VERTEX_POINT ( 'NONE', #2632 ) ;
#1147 = CARTESIAN_POINT ( 'NONE',  ( 0.000000000000000000, 0.000000000000000000, -20.00000000000000000 ) ) ;
#1148 = EDGE_CURVE ( 'NONE', #5556, #161, #4641, .T. ) ;
#1149 = FACE_OUTER_BOUND ( 'NONE', #4784, .T. ) ;
#1150 = CARTESIAN_POINT ( 'NONE',  ( 0.000000000000000000, 76.99999716619419132, 281.0000000000000000 ) ) ;
#1151 = CARTESIAN_POINT ( 'NONE',  ( 14.00000000000000000, 0.000000000000000000, 110.0000000000000000 ) ) ;
#1152 = ORIENTED_EDGE ( 'NONE', *, *, #3889, .F. ) ;
#1153 = CARTESIAN_POINT ( 'NONE',  ( 0.000000000000000000, 0.000000000000000000, 48.00000000000000000 ) ) ;
#1154 = AXIS2_PLACEMENT_3D ( 'NONE', #4809, #4253, #3814 ) ;
#1155 = ADVANCED_FACE ( 'NONE', ( #3600 ), #3489, .T. ) ;
#1156 = EDGE_CURVE ( 'NONE', #2487, #4674, #2007, .T. ) ;
#1157 = DIRECTION ( 'NONE',  ( -0.000000000000000000, -0.000000000000000000, -1.000000000000000000 ) ) ;
#1158 = CARTESIAN_POINT ( 'NONE',  ( -7.260561981364187290, 21.82400181508864634, 33.66843689838669462 ) ) ;
#1159 = LINE ( 'NONE', #1675, #2443 ) ;
#1160 = DIRECTION ( 'NONE',  ( -1.000000000000000000, 0.000000000000000000, 0.000000000000000000 ) ) ;
#1161 = ADVANCED_FACE ( 'NONE', ( #16, #1494 ), #4598, .F. ) ;
#1162 = ORIENTED_EDGE ( 'NONE', *, *, #3047, .F. ) ;
#1163 = VERTEX_POINT ( 'NONE', #1666 ) ;
#1164 = CYLINDRICAL_SURFACE ( 'NONE', #5723, 20.00000000000000000 ) ;
#1165 = PRODUCT_DEFINITION_SHAPE ( 'NONE', 'NONE',  #6374 ) ;
#1166 = DIRECTION ( 'NONE',  ( 1.000000000000000000, 0.000000000000000000, 0.000000000000000000 ) ) ;
#1167 = DIRECTION ( 'NONE',  ( 0.000000000000000000, 0.000000000000000000, 1.000000000000000000 ) ) ;
#1168 = ADVANCED_FACE ( 'NONE', ( #4632 ), #716, .T. ) ;
#1169 = DIRECTION ( 'NONE',  ( -0.000000000000000000, -0.000000000000000000, 1.000000000000000000 ) ) ;
#1170 = CARTESIAN_POINT ( 'NONE',  ( 17.00000000000000000, 69.00000000000000000, 110.0000000000000000 ) ) ;
#1171 = ORIENTED_EDGE ( 'NONE', *, *, #1817, .F. ) ;
#1172 = CARTESIAN_POINT ( 'NONE',  ( 44.00000000000008527, 13.41640786499836224, -65.00000000000000000 ) ) ;
#1173 = ADVANCED_FACE ( 'NONE', ( #5428, #4453 ), #3970, .F. ) ;
#1174 = DIRECTION ( 'NONE',  ( -1.000000000000000000, 0.000000000000000000, 0.000000000000000000 ) ) ;
#1175 = ORIENTED_EDGE ( 'NONE', *, *, #2540, .T. ) ;
#1176 = PLANE ( 'NONE',  #1444 ) ;
#1177 = ORIENTED_EDGE ( 'NONE', *, *, #1707, .T. ) ;
#1178 = APPLICATION_CONTEXT ( 'automotive_design' ) ;
#1179 = CARTESIAN_POINT ( 'NONE',  ( 17.00000000000000000, 25.00000000000000000, -30.00000000000000000 ) ) ;
#1180 =( NAMED_UNIT ( * ) SI_UNIT ( $, .STERADIAN. ) SOLID_ANGLE_UNIT ( ) );
#1181 = FACE_OUTER_BOUND ( 'NONE', #4413, .T. ) ;
#1182 = DIRECTION ( 'NONE',  ( -1.000000000000000000, -1.852483853906148286E-16, 0.000000000000000000 ) ) ;
#1183 = CYLINDRICAL_SURFACE ( 'NONE', #3807, 90.00000000000319744 ) ;
#1184 = VERTEX_POINT ( 'NONE', #2279 ) ;
#1185 = DIRECTION ( 'NONE',  ( 1.000000000000000000, 0.000000000000000000, 0.000000000000000000 ) ) ;
#1186 = CARTESIAN_POINT ( 'NONE',  ( -1.790150932673403750, 22.93126094008908566, 24.48831024192238814 ) ) ;
#1187 = CIRCLE ( 'NONE', #2629, 20.00000000000000000 ) ;
#1188 = VECTOR ( 'NONE', #5383, 1000.000000000000000 ) ;
#1189 = CARTESIAN_POINT ( 'NONE',  ( 10.32035317195591517, 22.78260342671239869, 6.723738260341699302 ) ) ;
#1190 = AXIS2_PLACEMENT_3D ( 'NONE', #4900, #5480, #2538 ) ;
#1191 = DIRECTION ( 'NONE',  ( -1.000000000000000000, 0.000000000000000000, 0.000000000000000000 ) ) ;
#1192 = ORIENTED_EDGE ( 'NONE', *, *, #2097, .F. ) ;
#1193 = ORIENTED_EDGE ( 'NONE', *, *, #5028, .F. ) ;
#1194 = EDGE_CURVE ( 'NONE', #2036, #1301, #4241, .T. ) ;
#1195 = ORIENTED_EDGE ( 'NONE', *, *, #669, .T. ) ;
#1196 = CARTESIAN_POINT ( 'NONE',  ( -19.25293315802950644, 8.385974291186926166, 12.00000000000000000 ) ) ;
#1197 = DIRECTION ( 'NONE',  ( -1.000000000000000000, 0.000000000000000000, 0.000000000000000000 ) ) ;
#1198 = CARTESIAN_POINT ( 'NONE',  ( 212.0000000000000284, 68.99999999999997158, 110.0000000000000000 ) ) ;
#1199 = LINE ( 'NONE', #3649, #2462 ) ;
#1200 = AXIS2_PLACEMENT_3D ( 'NONE', #4326, #3354, #6329 ) ;
#1201 = EDGE_CURVE ( 'NONE', #4878, #1470, #2683, .T. ) ;
#1202 = DIRECTION ( 'NONE',  ( 1.000000000000000000, 0.000000000000000000, 0.000000000000000000 ) ) ;
#1203 = EDGE_LOOP ( 'NONE', ( #4069, #6270, #2552, #5687 ) ) ;
#1204 = CIRCLE ( 'NONE', #1404, 12.50000000000001421 ) ;
#1205 = EDGE_CURVE ( 'NONE', #6074, #1416, #545, .T. ) ;
#1206 = FACE_OUTER_BOUND ( 'NONE', #1693, .T. ) ;
#1207 = ORIENTED_EDGE ( 'NONE', *, *, #1789, .F. ) ;
#1208 = DIRECTION ( 'NONE',  ( -0.000000000000000000, -0.000000000000000000, -1.000000000000000000 ) ) ;
#1209 = VERTEX_POINT ( 'NONE', #5669 ) ;
#1210=STYLED_ITEM('',(#6398),#4438);
#1211 = DIRECTION ( 'NONE',  ( -0.000000000000000000, -0.000000000000000000, -1.000000000000000000 ) ) ;
#1212 = UNCERTAINTY_MEASURE_WITH_UNIT (LENGTH_MEASURE( 1.000000000000000082E-05 ), #3670, 'distance_accuracy_value', 'NONE');
#1213 =( NAMED_UNIT ( * ) SI_UNIT ( $, .STERADIAN. ) SOLID_ANGLE_UNIT ( ) );
#1214 = DIRECTION ( 'NONE',  ( 1.000000000000000000, 0.000000000000000000, 0.000000000000000000 ) ) ;
#1215 = AXIS2_PLACEMENT_3D ( 'NONE', #140, #5423, #5483 ) ;
#1216 = FACE_OUTER_BOUND ( 'NONE', #1398, .T. ) ;
#1217 = FACE_OUTER_BOUND ( 'NONE', #4623, .T. ) ;
#1218 = EDGE_LOOP ( 'NONE', ( #2428, #21, #96, #6326 ) ) ;
#1219 = CARTESIAN_POINT ( 'NONE',  ( 0.000000000000000000, 0.000000000000000000, 44.00000000000000711 ) ) ;
#1220 = VECTOR ( 'NONE', #5462, 1000.000000000000000 ) ;
#1221 = AXIS2_PLACEMENT_3D ( 'NONE', #609, #3557, #4435 ) ;
#1222 = PRODUCT ( 'Part 32,4_Varsay\X2\0131\X0\lan', 'Part 32,4_Varsay\X2\0131\X0\lan', '', ( #5630 ) ) ;
#1223 = CARTESIAN_POINT ( 'NONE',  ( 21.00000000000000355, 2.571758278209442056E-15, -4.000000000000000000 ) ) ;
#1224 = CARTESIAN_POINT ( 'NONE',  ( 0.000000000000000000, 25.00000000000000000, 24.27501000028010125 ) ) ;
#1225 = AXIS2_PLACEMENT_3D ( 'NONE', #202, #5542, #5061 ) ;
#1226 = CARTESIAN_POINT ( 'NONE',  ( 15.99408614349810698, 19.21429697996681796, 0.000000000000000000 ) ) ;
#1227 = CARTESIAN_POINT ( 'NONE',  ( 7.059519746509402616, -21.88992045406459042, 34.31748813447425306 ) ) ;
#1228 = ORIENTED_EDGE ( 'NONE', *, *, #3047, .T. ) ;
#1229 = ORIENTED_EDGE ( 'NONE', *, *, #5316, .F. ) ;
#1230 = AXIS2_PLACEMENT_3D ( 'NONE', #5873, #2993, #2891 ) ;
#1231 = CARTESIAN_POINT ( 'NONE',  ( 9.185524248261779151E-16, 25.00000000000000000, 39.27501000028010480 ) ) ;
#1232 = EDGE_CURVE ( 'NONE', #5213, #306, #436, .T. ) ;
#1233 = CYLINDRICAL_SURFACE ( 'NONE', #585, 45.99999999999997868 ) ;
#1234 = DIRECTION ( 'NONE',  ( -1.000000000000000000, 0.000000000000000000, 0.000000000000000000 ) ) ;
#1235 = AXIS2_PLACEMENT_3D ( 'NONE', #4263, #1766, #6246 ) ;
#1236 = CYLINDRICAL_SURFACE ( 'NONE', #924, 12.50000000000000355 ) ;
#1237 = ORIENTED_EDGE ( 'NONE', *, *, #6018, .F. ) ;
#1238 = DIRECTION ( 'NONE',  ( 0.000000000000000000, -0.000000000000000000, 1.000000000000000000 ) ) ;
#1239 = ORIENTED_EDGE ( 'NONE', *, *, #1593, .T. ) ;
#1240 = AXIS2_PLACEMENT_3D ( 'NONE', #571, #24, #3103 ) ;
#1241 = EDGE_CURVE ( 'NONE', #2333, #5017, #1659, .T. ) ;
#1242 =( NAMED_UNIT ( * ) PLANE_ANGLE_UNIT ( ) SI_UNIT ( $, .RADIAN. ) );
#1243 = CARTESIAN_POINT ( 'NONE',  ( -15.23842499831731523, -17.23716120365648052, 1.424676953056493112 ) ) ;
#1244 = VERTEX_POINT ( 'NONE', #6221 ) ;
#1245 = DIRECTION ( 'NONE',  ( -1.000000000000000000, 0.000000000000000000, 0.000000000000000000 ) ) ;
#1246 = EDGE_CURVE ( 'NONE', #3894, #3208, #1559, .T. ) ;
#1247 = EDGE_CURVE ( 'NONE', #1008, #2696, #3309, .T. ) ;
#1248 = VECTOR ( 'NONE', #934, 1000.000000000000000 ) ;
#1249 = DIRECTION ( 'NONE',  ( 1.000000000000000000, 0.000000000000000000, 0.000000000000000000 ) ) ;
#1250 = DIRECTION ( 'NONE',  ( -0.000000000000000000, 0.000000000000000000, 1.000000000000000000 ) ) ;
#1251 = CARTESIAN_POINT ( 'NONE',  ( -8.000000000000021316, 1.481987083124922376E-15, 12.00000000000000000 ) ) ;
#1252 = DIRECTION ( 'NONE',  ( -0.000000000000000000, -0.000000000000000000, -1.000000000000000000 ) ) ;
#1253 = EDGE_CURVE ( 'NONE', #3554, #427, #1356, .T. ) ;
#1254 = LINE ( 'NONE', #2758, #931 ) ;
#1255 = ORIENTED_EDGE ( 'NONE', *, *, #1640, .T. ) ;
#1256 = SURFACE_STYLE_FILL_AREA ( #3707 ) ;
#1257 = ORIENTED_EDGE ( 'NONE', *, *, #2398, .T. ) ;
#1258 = CARTESIAN_POINT ( 'NONE',  ( 0.000000000000000000, 25.00000000000000000, 31.77501000028010125 ) ) ;
#1259 = CARTESIAN_POINT ( 'NONE',  ( -3.061616997868383043E-15, -25.00000000000000000, -65.00000000000000000 ) ) ;
#1260 = EDGE_CURVE ( 'NONE', #4309, #214, #4117, .T. ) ;
#1261 = EDGE_CURVE ( 'NONE', #3657, #2635, #3181, .T. ) ;
#1262 = CARTESIAN_POINT ( 'NONE',  ( 0.000000000000000000, 25.00000000000000000, 31.77501000028010125 ) ) ;
#1263 = VECTOR ( 'NONE', #4906, 1000.000000000000000 ) ;
#1264 = CARTESIAN_POINT ( 'NONE',  ( -1.331801922117356348E-14, -72.49991987048068154, 281.0000000000000000 ) ) ;
#1265 = ORIENTED_EDGE ( 'NONE', *, *, #77, .T. ) ;
#1266 = VERTEX_POINT ( 'NONE', #5159 ) ;
#1267 = FACE_OUTER_BOUND ( 'NONE', #2381, .T. ) ;
#1268 = FACE_OUTER_BOUND ( 'NONE', #6072, .T. ) ;
#1269 = CYLINDRICAL_SURFACE ( 'NONE', #5545, 22.67164836619070911 ) ;
#1270 = CARTESIAN_POINT ( 'NONE',  ( 0.000000000000000000, 120.0000000000000000, 0.000000000000000000 ) ) ;
#1271 = ORIENTED_EDGE ( 'NONE', *, *, #5310, .F. ) ;
#1272 = LINE ( 'NONE', #3201, #2649 ) ;
#1273 = VERTEX_POINT ( 'NONE', #1311 ) ;
#1274 = PRESENTATION_STYLE_ASSIGNMENT (( #4688 ) ) ;
#1275 = CARTESIAN_POINT ( 'NONE',  ( -11.95959904370095650, -19.64922365089178768, 5.386438528827848238 ) ) ;
#1276 = EDGE_LOOP ( 'NONE', ( #846, #2073, #5755, #2967 ) ) ;
#1277 = DIRECTION ( 'NONE',  ( -1.000000000000000000, 0.000000000000000000, 0.000000000000000000 ) ) ;
#1278 = VERTEX_POINT ( 'NONE', #843 ) ;
#1279 = DIRECTION ( 'NONE',  ( -1.000000000000000000, 0.000000000000000000, 0.000000000000000000 ) ) ;
#1280 =( LENGTH_UNIT ( ) NAMED_UNIT ( * ) SI_UNIT ( .MILLI., .METRE. ) );
#1281 = CARTESIAN_POINT ( 'NONE',  ( -12.50000000000001421, 120.0000000000000000, -4.000000000000000000 ) ) ;
#1282 = CYLINDRICAL_SURFACE ( 'NONE', #2740, 24.99999999999999289 ) ;
#1283 = CARTESIAN_POINT ( 'NONE',  ( -3.337067332043155865, -24.78046181229917266, 25.04046888573288143 ) ) ;
#1284 = EDGE_LOOP ( 'NONE', ( #2202, #3694 ) ) ;
#1285 = DIRECTION ( 'NONE',  ( 0.000000000000000000, -1.000000000000000000, 0.000000000000000000 ) ) ;
#1286 = ORIENTED_EDGE ( 'NONE', *, *, #5161, .F. ) ;
#1287 = CARTESIAN_POINT ( 'NONE',  ( 0.9839074788235817604, 24.98539006426129205, 39.22674605012093707 ) ) ;
#1288 = DIRECTION ( 'NONE',  ( -0.000000000000000000, -0.000000000000000000, 1.000000000000000000 ) ) ;
#1289 = AXIS2_PLACEMENT_3D ( 'NONE', #1147, #5092, #3055 ) ;
#1290 = AXIS2_PLACEMENT_3D ( 'NONE', #3928, #5410, #5832 ) ;
#1291 = CARTESIAN_POINT ( 'NONE',  ( -6.500000000000000000, 7.960204194457795477E-16, 47.00000000000000000 ) ) ;
#1292 = CARTESIAN_POINT ( 'NONE',  ( 3.765864371162155333, -24.71817793568963850, 25.27057431607724780 ) ) ;
#1293 = VERTEX_POINT ( 'NONE', #1281 ) ;
#1294 = VERTEX_POINT ( 'NONE', #6283 ) ;
#1295 = CARTESIAN_POINT ( 'NONE',  ( -2.655777422895189144, 24.85958502782042245, 24.75666344040547528 ) ) ;
#1296 = AXIS2_PLACEMENT_3D ( 'NONE', #556, #808, #2719 ) ;
#1297 = CARTESIAN_POINT ( 'NONE',  ( -20.00000000000000000, 0.000000000000000000, 51.00000000000002842 ) ) ;
#1298 = CARTESIAN_POINT ( 'NONE',  ( -17.00000000000000000, 2.081899558550500280E-15, -110.0000000000000000 ) ) ;
#1299 = DIRECTION ( 'NONE',  ( -0.000000000000000000, -1.000000000000000000, -0.000000000000000000 ) ) ;
#1300 = ORIENTED_EDGE ( 'NONE', *, *, #405, .F. ) ;
#1301 = VERTEX_POINT ( 'NONE', #4794 ) ;
#1302 = AXIS2_PLACEMENT_3D ( 'NONE', #3078, #2592, #5834 ) ;
#1303 = FILL_AREA_STYLE ('',( #3171 ) ) ;
#1304 = CARTESIAN_POINT ( 'NONE',  ( -0.9177768309508191891, -22.98591141273915639, 9.981795115530772478 ) ) ;
#1305 = LINE ( 'NONE', #3274, #5136 ) ;
#1306 = AXIS2_PLACEMENT_3D ( 'NONE', #3048, #1053, #30 ) ;
#1307 = CARTESIAN_POINT ( 'NONE',  ( 0.000000000000000000, 0.000000000000000000, 47.00000000000000711 ) ) ;
#1308 = EDGE_LOOP ( 'NONE', ( #1848, #5996 ) ) ;
#1309 = AXIS2_PLACEMENT_3D ( 'NONE', #5239, #3391, #2263 ) ;
#1310 = SHAPE_REPRESENTATION_RELATIONSHIP ( 'NONE' , 'NONE' ,  #1687, #103 ) ;
#1311 = CARTESIAN_POINT ( 'NONE',  ( 16.99999999999999645, -24.99999999999999645, -130.0000000000000000 ) ) ;
#1312 = DIRECTION ( 'NONE',  ( -0.000000000000000000, -0.000000000000000000, -1.000000000000000000 ) ) ;
#1313 = CIRCLE ( 'NONE', #6361, 45.99999999999997868 ) ;
#1314 = CARTESIAN_POINT ( 'NONE',  ( -6.734764818747084547, -24.07658780463482984, 35.11236497522016720 ) ) ;
#1315 = ORIENTED_EDGE ( 'NONE', *, *, #1970, .F. ) ;
#1316 = PRODUCT_DEFINITION_CONTEXT ( 'detailed design', #2911, 'design' ) ;
#1317 = LINE ( 'NONE', #3862, #4507 ) ;
#1318 = ORIENTED_EDGE ( 'NONE', *, *, #1367, .T. ) ;
#1319 = DIRECTION ( 'NONE',  ( 1.000000000000000000, 0.000000000000000000, 0.000000000000000000 ) ) ;
#1320 = CARTESIAN_POINT ( 'NONE',  ( 279.0000000000000000, 68.99999999999997158, 0.000000000000000000 ) ) ;
#1321 = AXIS2_PLACEMENT_3D ( 'NONE', #396, #3836, #879 ) ;
#1322 = ADVANCED_FACE ( 'NONE', ( #3214, #2720 ), #5638, .T. ) ;
#1323 = EDGE_CURVE ( 'NONE', #1030, #2050, #2693, .T. ) ;
#1324 = DIRECTION ( 'NONE',  ( 1.000000000000000000, 0.000000000000000000, 0.000000000000000000 ) ) ;
#1326 = EDGE_CURVE ( 'NONE', #3504, #453, #5168, .T. ) ;
#1325 = CARTESIAN_POINT ( 'NONE',  ( 4.953009495843455845, -24.50520187577543751, 26.13782778128491557 ) ) ;
#1327 = EDGE_LOOP ( 'NONE', ( #334, #1300, #3470, #1588, #296, #855 ) ) ;
#1328 = ORIENTED_EDGE ( 'NONE', *, *, #3925, .T. ) ;
#1329 = CARTESIAN_POINT ( 'NONE',  ( -6.737430854173823036, 24.07581932788625068, 28.44406090190431513 ) ) ;
#1330 = EDGE_CURVE ( 'NONE', #4113, #5536, #2383, .T. ) ;
#1331 = ADVANCED_FACE ( 'NONE', ( #809 ), #3702, .T. ) ;
#1332 = CIRCLE ( 'NONE', #2148, 166.8359700257217071 ) ;
#1333 = ADVANCED_BREP_SHAPE_REPRESENTATION ( '', ( #2488, #6349 ), #1412 ) ;
#1334 = CARTESIAN_POINT ( 'NONE',  ( 22.21770253897382474, 3.871672004622519037, -49.99999999999999289 ) ) ;
#1335 = DIRECTION ( 'NONE',  ( -0.000000000000000000, -0.000000000000000000, 1.000000000000000000 ) ) ;
#1336 = DIRECTION ( 'NONE',  ( -0.000000000000000000, -0.000000000000000000, -1.000000000000000000 ) ) ;
#1337 = VECTOR ( 'NONE', #589, 1000.000000000000000 ) ;
#1338 = VERTEX_POINT ( 'NONE', #4213 ) ;
#1339 = VERTEX_POINT ( 'NONE', #5701 ) ;
#1340 = ORIENTED_EDGE ( 'NONE', *, *, #3449, .T. ) ;
#1341 = PRODUCT_DEFINITION ( 'UNKNOWN', '', #3028, #4696 ) ;
#1342 = EDGE_CURVE ( 'NONE', #3225, #2036, #3246, .T. ) ;
#1343 = DIRECTION ( 'NONE',  ( -1.000000000000000000, 0.000000000000000000, 0.000000000000000000 ) ) ;
#1344 = AXIS2_PLACEMENT_3D ( 'NONE', #4410, #3020, #6341 ) ;
#1345 = CARTESIAN_POINT ( 'NONE',  ( -13.38016919228157420, 26.52751760200100861, 7.054451311141072267 ) ) ;
#1346 = VERTEX_POINT ( 'NONE', #524 ) ;
#1347 = DIRECTION ( 'NONE',  ( -0.000000000000000000, -0.000000000000000000, -1.000000000000000000 ) ) ;
#1348 = ORIENTED_EDGE ( 'NONE', *, *, #5078, .F. ) ;
#1349 = CARTESIAN_POINT ( 'NONE',  ( 0.000000000000000000, 25.00000000000000000, 24.27501000028010125 ) ) ;
#1350 = AXIS2_PLACEMENT_3D ( 'NONE', #1258, #2764, #2286 ) ;
#1351 = DIRECTION ( 'NONE',  ( 1.000000000000000000, 0.000000000000000000, 0.000000000000000000 ) ) ;
#1352 = CARTESIAN_POINT ( 'NONE',  ( 6.500000000000000000, 134.5953136438507158, 0.000000000000000000 ) ) ;
#1353 = LINE ( 'NONE', #3282, #3912 ) ;
#1354 = EDGE_LOOP ( 'NONE', ( #5339, #5786 ) ) ;
#1355 = CARTESIAN_POINT ( 'NONE',  ( 0.000000000000000000, 0.000000000000000000, 39.00000000000001421 ) ) ;
#1356 = CIRCLE ( 'NONE', #6300, 17.00000000000000000 ) ;
#1357 = ADVANCED_FACE ( 'NONE', ( #552 ), #5446, .T. ) ;
#1358 = CARTESIAN_POINT ( 'NONE',  ( 1.957493960826125923, 24.92801652726308248, 39.03205219918675795 ) ) ;
#1359 = LINE ( 'NONE', #726, #864 ) ;
#1360 = CYLINDRICAL_SURFACE ( 'NONE', #1832, 7.500000000000000000 ) ;
#1361 = CARTESIAN_POINT ( 'NONE',  ( 6.139315947428367615, -22.16738032098082911, 27.44370026704754650 ) ) ;
#1362 = ORIENTED_EDGE ( 'NONE', *, *, #4072, .F. ) ;
#1363 = ORIENTED_EDGE ( 'NONE', *, *, #32, .F. ) ;
#1364 = CARTESIAN_POINT ( 'NONE',  ( -4.955340051326917461, 24.50653216723387473, 37.42604413602551716 ) ) ;
#1365 = DIRECTION ( 'NONE',  ( -1.000000000000000000, 0.000000000000000000, 0.000000000000000000 ) ) ;
#1366 = DIRECTION ( 'NONE',  ( -1.000000000000000000, 0.000000000000000000, 0.000000000000000000 ) ) ;
#1367 = EDGE_CURVE ( 'NONE', #5659, #3460, #487, .T. ) ;
#1368 = DIRECTION ( 'NONE',  ( -0.000000000000000000, 0.000000000000000000, 1.000000000000000000 ) ) ;
#1369 = ORIENTED_EDGE ( 'NONE', *, *, #2653, .T. ) ;
#1370 = ORIENTED_EDGE ( 'NONE', *, *, #3127, .F. ) ;
#1371 = VECTOR ( 'NONE', #6131, 1000.000000000000000 ) ;
#1372 = CARTESIAN_POINT ( 'NONE',  ( -21.00000000000000355, 0.000000000000000000, -4.000000000000000000 ) ) ;
#1373 = CYLINDRICAL_SURFACE ( 'NONE', #1743, 17.79053956122086078 ) ;
#1374 = DIRECTION ( 'NONE',  ( -0.000000000000000000, 0.000000000000000000, -1.000000000000000000 ) ) ;
#1375 = EDGE_LOOP ( 'NONE', ( #1991, #4978 ) ) ;
#1376 = FACE_OUTER_BOUND ( 'NONE', #4087, .T. ) ;
#1377 = CARTESIAN_POINT ( 'NONE',  ( -4.240673024049072204, -22.60901396202200075, 25.57291330172528987 ) ) ;
#1378 = CARTESIAN_POINT ( 'NONE',  ( -17.00000000000000000, 25.00000000000000000, -195.0000000000000000 ) ) ;
#1379 = DIRECTION ( 'NONE',  ( 0.000000000000000000, 0.000000000000000000, 1.000000000000000000 ) ) ;
#1380 = EDGE_LOOP ( 'NONE', ( #4030, #4690 ) ) ;
#1381 = CARTESIAN_POINT ( 'NONE',  ( -16.23652742703190199, -37.28747423195189015, -175.0000000000000284 ) ) ;
#1382 = CARTESIAN_POINT ( 'NONE',  ( -15.82602517378898987, 37.28747423195201094, 0.000000000000000000 ) ) ;
#1383 = CARTESIAN_POINT ( 'NONE',  ( 6.500000000000000000, 130.6770782520313219, 12.00000000000000000 ) ) ;
#1384 = CARTESIAN_POINT ( 'NONE',  ( 3.122849337825750617E-15, -17.00000000000000000, -20.00000000000000000 ) ) ;
#1385 = CARTESIAN_POINT ( 'NONE',  ( 7.018581182383306860, -23.99477090726734829, 29.12000203626550032 ) ) ;
#1386 = VERTEX_POINT ( 'NONE', #4959 ) ;
#1387 = DIRECTION ( 'NONE',  ( -0.000000000000000000, -0.000000000000000000, -1.000000000000000000 ) ) ;
#1388 = ORIENTED_EDGE ( 'NONE', *, *, #1436, .F. ) ;
#1389 =( REPRESENTATION_RELATIONSHIP ('NONE','NONE', #632, #3711 ) REPRESENTATION_RELATIONSHIP_WITH_TRANSFORMATION ( #868 )SHAPE_REPRESENTATION_RELATIONSHIP( ) );
#1390 = DIRECTION ( 'NONE',  ( 0.000000000000000000, 0.000000000000000000, 1.000000000000000000 ) ) ;
#1391 = VECTOR ( 'NONE', #4591, 1000.000000000000000 ) ;
#1392 = CARTESIAN_POINT ( 'NONE',  ( 2.012341796004660122, 25.00000000000000000, 39.00000000000001421 ) ) ;
#1393 = CARTESIAN_POINT ( 'NONE',  ( -22.00000000000000000, 0.000000000000000000, 50.00000000000000711 ) ) ;
#1394 = CIRCLE ( 'NONE', #6237, 7.500000000000000000 ) ;
#1395 = EDGE_CURVE ( 'NONE', #3949, #258, #2475, .T. ) ;
#1396 = CARTESIAN_POINT ( 'NONE',  ( -17.00000000000000355, -24.99999999999999645, -65.00000000000000000 ) ) ;
#1397 = ORIENTED_EDGE ( 'NONE', *, *, #5347, .T. ) ;
#1398 = EDGE_LOOP ( 'NONE', ( #2607, #2726, #1171, #805 ) ) ;
#1399 = CARTESIAN_POINT ( 'NONE',  ( 0.000000000000000000, 0.000000000000000000, 44.00000000000000711 ) ) ;
#1400 = AXIS2_PLACEMENT_3D ( 'NONE', #5589, #373, #1948 ) ;
#1401 = VECTOR ( 'NONE', #183, 1000.000000000000000 ) ;
#1402 = FACE_OUTER_BOUND ( 'NONE', #4776, .T. ) ;
#1403 = ADVANCED_FACE ( 'NONE', ( #2507, #3832 ), #2916, .F. ) ;
#1404 = AXIS2_PLACEMENT_3D ( 'NONE', #1696, #137, #6120 ) ;
#1405 = CARTESIAN_POINT ( 'NONE',  ( 6.736323264042102466, -24.07882193050101449, 8.680799421305112062 ) ) ;
#1406 = EDGE_CURVE ( 'NONE', #1569, #2268, #1480, .T. ) ;
#1407 = ORIENTED_EDGE ( 'NONE', *, *, #699, .T. ) ;
#1408 = ORIENTED_EDGE ( 'NONE', *, *, #1052, .F. ) ;
#1409 = DIRECTION ( 'NONE',  ( 1.000000000000000000, 0.000000000000000000, 0.000000000000000000 ) ) ;
#1410 = ADVANCED_FACE ( 'NONE', ( #5803 ), #3891, .T. ) ;
#1411 = EDGE_CURVE ( 'NONE', #1070, #5642, #1592, .T. ) ;
#1412 =( GEOMETRIC_REPRESENTATION_CONTEXT ( 3 ) GLOBAL_UNCERTAINTY_ASSIGNED_CONTEXT ( ( #3212 ) ) GLOBAL_UNIT_ASSIGNED_CONTEXT ( ( #486, #1870, #4793 ) ) REPRESENTATION_CONTEXT ( 'NONE', 'WORKASPACE' ) );
#1413 = CARTESIAN_POINT ( 'NONE',  ( -0.9006954679665252206, -22.98346407483541753, 24.32584948309267148 ) ) ;
#1414 = DIRECTION ( 'NONE',  ( 1.000000000000000000, 0.000000000000000000, 0.000000000000000000 ) ) ;
#1415 = DIRECTION ( 'NONE',  ( 0.000000000000000000, 0.000000000000000000, 1.000000000000000000 ) ) ;
#1416 = VERTEX_POINT ( 'NONE', #4407 ) ;
#1417 = FACE_OUTER_BOUND ( 'NONE', #2458, .T. ) ;
#1418 = VECTOR ( 'NONE', #6236, 1000.000000000000000 ) ;
#1419 = DIRECTION ( 'NONE',  ( 0.000000000000000000, 0.000000000000000000, -1.000000000000000000 ) ) ;
#1420 = AXIS2_PLACEMENT_3D ( 'NONE', #5660, #3868, #1425 ) ;
#1421 = AXIS2_PLACEMENT_3D ( 'NONE', #2212, #332, #4733 ) ;
#1422 = CARTESIAN_POINT ( 'NONE',  ( 0.000000000000000000, 69.00000000000000000, 110.0000000000000000 ) ) ;
#1423 = CARTESIAN_POINT ( 'NONE',  ( 1.568280873051609348, -22.94756140746006778, 24.43729500028611312 ) ) ;
#1424 = ORIENTED_EDGE ( 'NONE', *, *, #1799, .F. ) ;
#1425 = DIRECTION ( 'NONE',  ( -1.000000000000000000, 0.000000000000000000, 0.000000000000000000 ) ) ;
#1426 = CIRCLE ( 'NONE', #5021, 46.00000000000000000 ) ;
#1427 = CARTESIAN_POINT ( 'NONE',  ( 17.00000000000000000, 0.000000000000000000, -273.0000000000000000 ) ) ;
#1428 = DIRECTION ( 'NONE',  ( 1.836970198721029194E-16, 1.000000000000000000, 0.000000000000000000 ) ) ;
#1429 = DIRECTION ( 'NONE',  ( 0.000000000000000000, 0.000000000000000000, -1.000000000000000000 ) ) ;
#1430 = DIRECTION ( 'NONE',  ( 0.000000000000000000, 0.000000000000000000, 1.000000000000000000 ) ) ;
#1431 = CIRCLE ( 'NONE', #5029, 22.00000000000000000 ) ;
#1432 = CARTESIAN_POINT ( 'NONE',  ( -2.012341796004660122, 25.00000000000000000, 39.00000000000001421 ) ) ;
#1433 = VERTEX_POINT ( 'NONE', #2956 ) ;
#1434 = ORIENTED_EDGE ( 'NONE', *, *, #3467, .T. ) ;
#1435 = AXIS2_PLACEMENT_3D ( 'NONE', #5657, #4648, #3104 ) ;
#1436 = EDGE_CURVE ( 'NONE', #1896, #6074, #5858, .T. ) ;
#1437 = AXIS2_PLACEMENT_3D ( 'NONE', #2023, #577, #5960 ) ;
#1438 = LINE ( 'NONE', #1919, #3922 ) ;
#1439 = CONTEXT_DEPENDENT_SHAPE_REPRESENTATION ( #3156, #3121 ) ;
#1440 = LINE ( 'NONE', #3880, #4932 ) ;
#1441 = CARTESIAN_POINT ( 'NONE',  ( -9.287558414957933550, -23.21379839259252975, 7.388795739543621899 ) ) ;
#1442 = ORIENTED_EDGE ( 'NONE', *, *, #5705, .T. ) ;
#1443 = EDGE_CURVE ( 'NONE', #1773, #116, #1861, .T. ) ;
#1444 = AXIS2_PLACEMENT_3D ( 'NONE', #677, #225, #648 ) ;
#1445 = CARTESIAN_POINT ( 'NONE',  ( -16.23652742703190199, -37.28747423195189015, -160.0000000000000284 ) ) ;
#1446 = DIRECTION ( 'NONE',  ( 1.000000000000000000, -2.225818823800548493E-16, -4.776461258691548054E-16 ) ) ;
#1447 = DIRECTION ( 'NONE',  ( -0.000000000000000000, -0.000000000000000000, 1.000000000000000000 ) ) ;
#1448 = CARTESIAN_POINT ( 'NONE',  ( 17.05141243254543681, -12.25762350764760455, 0.000000000000000000 ) ) ;
#1449 = EDGE_CURVE ( 'NONE', #3460, #6200, #1143, .T. ) ;
#1450 = CYLINDRICAL_SURFACE ( 'NONE', #1961, 7.500000000000000000 ) ;
#1451 = ORIENTED_EDGE ( 'NONE', *, *, #2077, .T. ) ;
#1452 = EDGE_CURVE ( 'NONE', #2909, #4309, #2423, .T. ) ;
#1453 = CARTESIAN_POINT ( 'NONE',  ( 1.353316873173489032, 19.96515186930334096, 39.18355504947043499 ) ) ;
#1454 = AXIS2_PLACEMENT_3D ( 'NONE', #6194, #880, #2217 ) ;
#1455 = VECTOR ( 'NONE', #4398, 1000.000000000000000 ) ;
#1456 = FACE_BOUND ( 'NONE', #2815, .T. ) ;
#1457 = EDGE_CURVE ( 'NONE', #633, #6022, #1054, .T. ) ;
#1458 = CARTESIAN_POINT ( 'NONE',  ( -12.54137761259614159, 29.87368101119750818, 2.025772336917470717 ) ) ;
#1459 = CARTESIAN_POINT ( 'NONE',  ( 0.4915545007834231650, -24.99637963107062433, 39.26296923598712851 ) ) ;
#1460 = VERTEX_POINT ( 'NONE', #4984 ) ;
#1461 = PRODUCT_RELATED_PRODUCT_CATEGORY ( 'part', '', ( #2145 ) ) ;
#1462 = SURFACE_STYLE_FILL_AREA ( #1552 ) ;
#1463 = ORIENTED_EDGE ( 'NONE', *, *, #3449, .F. ) ;
#1464 = DIRECTION ( 'NONE',  ( 0.000000000000000000, 0.000000000000000000, -1.000000000000000000 ) ) ;
#1465 = ADVANCED_FACE ( 'NONE', ( #2530 ), #2932, .T. ) ;
#1466 = CARTESIAN_POINT ( 'NONE',  ( -44.00000000000000000, -13.41640786499873172, -225.0000000000000000 ) ) ;
#1467 = PRODUCT_DEFINITION_CONTEXT ( 'detailed design', #2253, 'design' ) ;
#1468 = FACE_OUTER_BOUND ( 'NONE', #4320, .T. ) ;
#1469 = DIRECTION ( 'NONE',  ( 0.000000000000000000, 0.000000000000000000, -1.000000000000000000 ) ) ;
#1470 = VERTEX_POINT ( 'NONE', #2599 ) ;
#1471 = ORIENTED_EDGE ( 'NONE', *, *, #5559, .F. ) ;
#1472 = ORIENTED_EDGE ( 'NONE', *, *, #1654, .T. ) ;
#1473 = LINE ( 'NONE', #5823, #3715 ) ;
#1474 = CARTESIAN_POINT ( 'NONE',  ( 147.0000000000000284, 69.00000000000000000, 110.0000000000000000 ) ) ;
#1475 = AXIS2_PLACEMENT_3D ( 'NONE', #537, #5369, #3942 ) ;
#1476 = DIRECTION ( 'NONE',  ( 1.000000000000000000, 0.000000000000000000, 0.000000000000000000 ) ) ;
#1477 = ORIENTED_EDGE ( 'NONE', *, *, #529, .T. ) ;
#1478 = DIRECTION ( 'NONE',  ( -1.000000000000000000, 0.000000000000000000, 0.000000000000000000 ) ) ;
#1479 = SHAPE_REPRESENTATION_RELATIONSHIP ( 'NONE' , 'NONE' ,  #5606, #1333 ) ;
#1480 = LINE ( 'NONE', #4826, #994 ) ;
#1481 = CARTESIAN_POINT ( 'NONE',  ( 8.000000000000001776, 100.3953136438507272, 5.999999999999999112 ) ) ;
#1482 = EDGE_LOOP ( 'NONE', ( #2941, #5890, #5376, #3270 ) ) ;
#1483 = CARTESIAN_POINT ( 'NONE',  ( -6.500000000000000000, 134.5953136438507158, 0.000000000000000000 ) ) ;
#1484 = CARTESIAN_POINT ( 'NONE',  ( 0.000000000000000000, 0.000000000000000000, 301.0000000000000568 ) ) ;
#1485 = CYLINDRICAL_SURFACE ( 'NONE', #400, 24.99999999999999289 ) ;
#1486 = EDGE_CURVE ( 'NONE', #3225, #6319, #5007, .T. ) ;
#1487 = CARTESIAN_POINT ( 'NONE',  ( -19.00000000000000000, 0.000000000000000000, 23.00000000000000000 ) ) ;
#1488 = VERTEX_POINT ( 'NONE', #5994 ) ;
#1489 = CARTESIAN_POINT ( 'NONE',  ( 0.000000000000000000, -25.00000000000000000, 301.0000000000000568 ) ) ;
#1490 = SHAPE_REPRESENTATION ( 'Part 32,2_Varsay\X2\0131\X0\lan', ( #6349 ), #4174 ) ;
#1491 = CARTESIAN_POINT ( 'NONE',  ( 13.38016919228157420, 26.52751760200101216, 7.054451311141071379 ) ) ;
#1492 = CARTESIAN_POINT ( 'NONE',  ( 174.7835321302054865, 68.75545066608756883, 12.00000000000000000 ) ) ;
#1493 = EDGE_CURVE ( 'NONE', #4451, #5912, #169, .T. ) ;
#1494 = FACE_BOUND ( 'NONE', #4888, .T. ) ;
#1495 = CYLINDRICAL_SURFACE ( 'NONE', #6144, 17.00000000000000000 ) ;
#1496 = LINE ( 'NONE', #4643, #102 ) ;
#1497 = ORIENTED_EDGE ( 'NONE', *, *, #118, .T. ) ;
#1498 = ORIENTED_EDGE ( 'NONE', *, *, #3610, .F. ) ;
#1499 = ORIENTED_EDGE ( 'NONE', *, *, #2188, .F. ) ;
#1500 = CARTESIAN_POINT ( 'NONE',  ( 13.05910636442709993, 27.77388734089489120, 2.967234880352092929 ) ) ;
#1501 = VECTOR ( 'NONE', #1288, 1000.000000000000000 ) ;
#1502 = DIRECTION ( 'NONE',  ( -0.000000000000000000, -0.000000000000000000, -1.000000000000000000 ) ) ;
#1503 = VECTOR ( 'NONE', #4518, 1000.000000000000000 ) ;
#1504 = DIRECTION ( 'NONE',  ( 0.000000000000000000, -1.000000000000000000, 0.000000000000000000 ) ) ;
#1505 = EDGE_LOOP ( 'NONE', ( #2978, #544, #356, #470, #751, #2174 ) ) ;
#1506 = AXIS2_PLACEMENT_3D ( 'NONE', #3371, #448, #2343 ) ;
#1507 = APPLICATION_PROTOCOL_DEFINITION ( 'draft international standard', 'automotive_design', 1998, #2253 ) ;
#1508 = CARTESIAN_POINT ( 'NONE',  ( -7.267038029898874818, -21.82227126734110456, 29.86717584346564180 ) ) ;
#1509 = DIRECTION ( 'NONE',  ( 0.000000000000000000, 0.000000000000000000, -1.000000000000000000 ) ) ;
#1510 = ORIENTED_EDGE ( 'NONE', *, *, #3541, .F. ) ;
#1511 = CARTESIAN_POINT ( 'NONE',  ( -7.182657412981705209E-17, 20.00000000000000711, 39.27501000028011902 ) ) ;
#1512 = CIRCLE ( 'NONE', #1302, 166.8359700257217071 ) ;
#1513 = DIRECTION ( 'NONE',  ( 1.000000000000000000, 0.000000000000000000, 0.000000000000000000 ) ) ;
#1514 =( REPRESENTATION_RELATIONSHIP ('NONE','NONE', #632, #1687 ) REPRESENTATION_RELATIONSHIP_WITH_TRANSFORMATION ( #1723 )SHAPE_REPRESENTATION_RELATIONSHIP( ) );
#1515 = CARTESIAN_POINT ( 'NONE',  ( 0.000000000000000000, 120.0000000000000000, 16.00000000000000000 ) ) ;
#1516 = CIRCLE ( 'NONE', #1012, 17.00000000000000000 ) ;
#1517 = CARTESIAN_POINT ( 'NONE',  ( 8.000000000000021316, 1.481987083124922376E-15, 0.000000000000000000 ) ) ;
#1518 = VERTEX_POINT ( 'NONE', #4102 ) ;
#1519 = CARTESIAN_POINT ( 'NONE',  ( 174.7835321302054865, 68.75545066608756883, 1.999999999999994893 ) ) ;
#1520 = CARTESIAN_POINT ( 'NONE',  ( 12.54049055679404212, 29.87738611749457718, 9.974675204776747961 ) ) ;
#1521 = FACE_OUTER_BOUND ( 'NONE', #2504, .T. ) ;
#1522 = EDGE_CURVE ( 'NONE', #3828, #3948, #160, .T. ) ;
#1523 = AXIS2_PLACEMENT_3D ( 'NONE', #6284, #6188, #2757 ) ;
#1524 = DIRECTION ( 'NONE',  ( 1.000000000000000000, 0.000000000000000000, 0.000000000000000000 ) ) ;
#1525 = ADVANCED_FACE ( 'NONE', ( #1662 ), #6083, .T. ) ;
#1526 = CARTESIAN_POINT ( 'NONE',  ( 16.23652742703164975, 37.28747423195200383, -30.00000000000000000 ) ) ;
#1527 = CYLINDRICAL_SURFACE ( 'NONE', #2663, 25.00000000000000000 ) ;
#1528 = VECTOR ( 'NONE', #1908, 1000.000000000000000 ) ;
#1529 = ORIENTED_EDGE ( 'NONE', *, *, #5548, .F. ) ;
#1530 = EDGE_LOOP ( 'NONE', ( #3583, #5534, #2892, #3112, #6191, #6092 ) ) ;
#1531 = EDGE_CURVE ( 'NONE', #2677, #5616, #3140, .T. ) ;
#1532 = AXIS2_PLACEMENT_3D ( 'NONE', #1153, #4570, #3186 ) ;
#1533 = DIRECTION ( 'NONE',  ( 1.000000000000000000, 0.000000000000000000, 0.000000000000000000 ) ) ;
#1534 = CARTESIAN_POINT ( 'NONE',  ( 0.000000000000000000, 0.000000000000000000, -115.0000000000000000 ) ) ;
#1535 = VECTOR ( 'NONE', #3068, 1000.000000000000000 ) ;
#1536 = CARTESIAN_POINT ( 'NONE',  ( -4.673148220383225748, -24.56288069930688067, 9.380541037249376046 ) ) ;
#1537 = VERTEX_POINT ( 'NONE', #3535 ) ;
#1538 = VECTOR ( 'NONE', #993, 1000.000000000000000 ) ;
#1539 = EDGE_CURVE ( 'NONE', #3044, #3551, #4683, .T. ) ;
#1540 = AXIS2_PLACEMENT_3D ( 'NONE', #1749, #145, #2190 ) ;
#1541 = CARTESIAN_POINT ( 'NONE',  ( -7.071085268539269109, -21.88683845148715079, 34.31457501568616664 ) ) ;
#1542 = DIRECTION ( 'NONE',  ( -1.000000000000000000, 0.000000000000000000, 0.000000000000000000 ) ) ;
#1543 = ORIENTED_EDGE ( 'NONE', *, *, #3879, .T. ) ;
#1544 = CARTESIAN_POINT ( 'NONE',  ( 0.000000000000000000, 0.000000000000000000, 281.0000000000000000 ) ) ;
#1545 = VECTOR ( 'NONE', #1866, 1000.000000000000000 ) ;
#1546 = CARTESIAN_POINT ( 'NONE',  ( 0.000000000000000000, 0.000000000000000000, -225.0000000000000000 ) ) ;
#1547 = VECTOR ( 'NONE', #3052, 1000.000000000000000 ) ;
#1548 = FACE_OUTER_BOUND ( 'NONE', #3286, .T. ) ;
#1549 = CARTESIAN_POINT ( 'NONE',  ( 0.9837646592764097697, -24.98184996318330775, 39.21432222910940624 ) ) ;
#1550 = ORIENTED_EDGE ( 'NONE', *, *, #664, .T. ) ;
#1551 = CLOSED_SHELL ( 'NONE', ( #4759, #1798, #3501, #1525, #5370, #1064, #1465, #4073 ) ) ;
#1552 = FILL_AREA_STYLE ('',( #2066 ) ) ;
#1553 = CARTESIAN_POINT ( 'NONE',  ( 13.15428815592193956, 27.40009807703880540, 8.663997969339835237 ) ) ;
#1554 = CARTESIAN_POINT ( 'NONE',  ( 5.103812965180195782, 22.42723062334006556, 26.27493091522155666 ) ) ;
#1555 = DIRECTION ( 'NONE',  ( 1.852483853906148040E-16, 1.000000000000000000, 1.239088197126290570E-16 ) ) ;
#1556 = DIRECTION ( 'NONE',  ( 0.000000000000000000, 0.000000000000000000, 1.000000000000000000 ) ) ;
#1557 = VERTEX_POINT ( 'NONE', #4559 ) ;
#1558 = ORIENTED_EDGE ( 'NONE', *, *, #3748, .T. ) ;
#1559 = CIRCLE ( 'NONE', #4021, 89.87058297576894006 ) ;
#1560 = CARTESIAN_POINT ( 'NONE',  ( 23.00000000000000000, 2.816687638038912352E-15, 0.000000000000000000 ) ) ;
#1561 = DIRECTION ( 'NONE',  ( 1.000000000000000000, 0.000000000000000000, 0.000000000000000000 ) ) ;
#1562 = DIRECTION ( 'NONE',  ( -1.000000000000000000, 0.000000000000000000, 0.000000000000000000 ) ) ;
#1563 = DIRECTION ( 'NONE',  ( 1.000000000000000000, 0.000000000000000000, 0.000000000000000000 ) ) ;
#1564 = ORIENTED_EDGE ( 'NONE', *, *, #5084, .T. ) ;
#1565 = PRODUCT_CONTEXT ( 'NONE', #867, 'mechanical' ) ;
#1566 = DIRECTION ( 'NONE',  ( 0.000000000000000000, -0.000000000000000000, -1.000000000000000000 ) ) ;
#1567 = AXIS2_PLACEMENT_3D ( 'NONE', #5041, #4123, #2679 ) ;
#1568 = DIRECTION ( 'NONE',  ( -0.000000000000000000, -0.000000000000000000, -1.000000000000000000 ) ) ;
#1569 = VERTEX_POINT ( 'NONE', #2113 ) ;
#1570 = ORIENTED_EDGE ( 'NONE', *, *, #968, .F. ) ;
#1571 = CYLINDRICAL_SURFACE ( 'NONE', #2421, 46.00000000000000000 ) ;
#1572 = CARTESIAN_POINT ( 'NONE',  ( 0.000000000000000000, 0.000000000000000000, -20.00000000000000000 ) ) ;
#1573 = FACE_BOUND ( 'NONE', #4746, .T. ) ;
#1574 = VERTEX_POINT ( 'NONE', #1595 ) ;
#1575 = CARTESIAN_POINT ( 'NONE',  ( 11.04889961723839775, 20.18459349909284839, 6.176241220338072324 ) ) ;
#1576 = CARTESIAN_POINT ( 'NONE',  ( 279.0000000000000000, 14.00000000000000000, 110.0000000000000000 ) ) ;
#1577 = CARTESIAN_POINT ( 'NONE',  ( 3.474965785108256267, 22.73929270720903872, 25.11363447059788712 ) ) ;
#1578 = CARTESIAN_POINT ( 'NONE',  ( 13.14183123006966980, -39.58265509608656174, -110.0000000000000000 ) ) ;
#1579 = DIRECTION ( 'NONE',  ( -1.000000000000000000, 0.000000000000000000, 0.000000000000000000 ) ) ;
#1580 = ORIENTED_EDGE ( 'NONE', *, *, #4589, .F. ) ;
#1581 = ORIENTED_EDGE ( 'NONE', *, *, #5069, .F. ) ;
#1582 = FACE_OUTER_BOUND ( 'NONE', #3616, .T. ) ;
#1583 = CARTESIAN_POINT ( 'NONE',  ( 16.23652742703164620, 37.28747423195200383, -240.0000000000000000 ) ) ;
#1584 = EDGE_CURVE ( 'NONE', #5526, #4, #5827, .T. ) ;
#1585 = DIRECTION ( 'NONE',  ( 1.000000000000000000, 0.000000000000000000, 0.000000000000000000 ) ) ;
#1586 = DIRECTION ( 'NONE',  ( 1.000000000000000000, 0.000000000000000000, 0.000000000000000000 ) ) ;
#1587 = DIRECTION ( 'NONE',  ( -0.000000000000000000, -0.000000000000000000, 1.000000000000000000 ) ) ;
#1588 = ORIENTED_EDGE ( 'NONE', *, *, #2011, .T. ) ;
#1589 = AXIS2_PLACEMENT_3D ( 'NONE', #907, #3935, #2999 ) ;
#1590 = APPLICATION_CONTEXT ( 'automotive_design' ) ;
#1591 = EDGE_CURVE ( 'NONE', #1163, #3913, #3969, .T. ) ;
#1592 = CIRCLE ( 'NONE', #1290, 7.500000000000000000 ) ;
#1593 = EDGE_CURVE ( 'NONE', #1416, #6038, #5567, .T. ) ;
#1594 = PRODUCT_CONTEXT ( 'NONE', #4893, 'mechanical' ) ;
#1595 = CARTESIAN_POINT ( 'NONE',  ( 147.0000000000000284, 69.00000000000000000, 0.000000000000000000 ) ) ;
#1596 = EDGE_CURVE ( 'NONE', #5642, #1070, #4267, .T. ) ;
#1597 = DIRECTION ( 'NONE',  ( -0.000000000000000000, -0.000000000000000000, 1.000000000000000000 ) ) ;
#1598 = ORIENTED_EDGE ( 'NONE', *, *, #5920, .F. ) ;
#1599 = ADVANCED_FACE ( 'NONE', ( #1206 ), #1690, .T. ) ;
#1600 = EDGE_CURVE ( 'NONE', #4629, #4999, #6335, .T. ) ;
#1601 = VECTOR ( 'NONE', #5254, 1000.000000000000000 ) ;
#1602 = DIRECTION ( 'NONE',  ( -0.000000000000000000, -0.000000000000000000, -1.000000000000000000 ) ) ;
#1603 = AXIS2_PLACEMENT_3D ( 'NONE', #5398, #2810, #4811 ) ;
#1604 = DIRECTION ( 'NONE',  ( 0.000000000000000000, -1.000000000000000000, 0.000000000000000000 ) ) ;
#1605 = DIRECTION ( 'NONE',  ( -0.000000000000000000, -0.000000000000000000, -1.000000000000000000 ) ) ;
#1606 = ORIENTED_EDGE ( 'NONE', *, *, #1443, .F. ) ;
#1607 = CIRCLE ( 'NONE', #2536, 17.00000000000000000 ) ;
#1608 = CARTESIAN_POINT ( 'NONE',  ( -8.270741877429188094, 21.47680860501242961, 7.983294599549966897 ) ) ;
#1609 = DIRECTION ( 'NONE',  ( 1.000000000000000000, 0.000000000000000000, 0.000000000000000000 ) ) ;
#1610 = CARTESIAN_POINT ( 'NONE',  ( 7.058581574212176690, 21.89022081680645826, 29.23014371996821481 ) ) ;
#1611 = EDGE_CURVE ( 'NONE', #3765, #394, #5620, .T. ) ;
#1612 = EDGE_CURVE ( 'NONE', #3307, #2452, #3646, .T. ) ;
#1613 = VECTOR ( 'NONE', #3858, 1000.000000000000000 ) ;
#1614 = CARTESIAN_POINT ( 'NONE',  ( 7.831318214037675141, 23.74511713421663472, 8.189156644668285523 ) ) ;
#1615 = LINE ( 'NONE', #1264, #4002 ) ;
#1616 = ORIENTED_EDGE ( 'NONE', *, *, #4955, .T. ) ;
#1617 = EDGE_LOOP ( 'NONE', ( #5605, #923, #6262, #1580 ) ) ;
#1618 = ORIENTED_EDGE ( 'NONE', *, *, #1449, .F. ) ;
#1619 = LINE ( 'NONE', #856, #4240 ) ;
#1620 = CARTESIAN_POINT ( 'NONE',  ( -6.500000000000000000, 0.000000000000000000, 12.00000000000000000 ) ) ;
#1621 = LINE ( 'NONE', #5561, #1114 ) ;
#1622 = AXIS2_PLACEMENT_3D ( 'NONE', #5926, #420, #2374 ) ;
#1623 = DIRECTION ( 'NONE',  ( 1.000000000000000000, 0.000000000000000000, 0.000000000000000000 ) ) ;
#1624 = CARTESIAN_POINT ( 'NONE',  ( 18.00000000000001421, 30.39531364385072010, 5.999999999999990230 ) ) ;
#1625 = ORIENTED_EDGE ( 'NONE', *, *, #191, .F. ) ;
#1626 = EDGE_CURVE ( 'NONE', #434, #81, #6028, .T. ) ;
#1627 = MECHANICAL_DESIGN_GEOMETRIC_PRESENTATION_REPRESENTATION (  '', ( #6060 ), #5240 ) ;
#1628 = CARTESIAN_POINT ( 'NONE',  ( -98.68819482895224837, 82.87638965790608836, 281.2329880893517497 ) ) ;
#1629 = CARTESIAN_POINT ( 'NONE',  ( -6.710385028064199453, -21.99961506306615178, 35.13225475196805547 ) ) ;
#1630 = EDGE_CURVE ( 'NONE', #146, #1019, #5206, .T. ) ;
#1631 = ORIENTED_EDGE ( 'NONE', *, *, #5363, .T. ) ;
#1632 = AXIS2_PLACEMENT_3D ( 'NONE', #2787, #2984, #1562 ) ;
#1633 = CYLINDRICAL_SURFACE ( 'NONE', #5777, 7.500000000000000000 ) ;
#1634 = ORIENTED_EDGE ( 'NONE', *, *, #5625, .T. ) ;
#1635 = AXIS2_PLACEMENT_3D ( 'NONE', #4782, #957, #6330 ) ;
#1636 = PLANE ( 'NONE',  #4478 ) ;
#1637 = DIRECTION ( 'NONE',  ( 0.000000000000000000, 0.000000000000000000, 1.000000000000000000 ) ) ;
#1638 = ADVANCED_FACE ( 'NONE', ( #5617 ), #2076, .F. ) ;
#1639 = LINE ( 'NONE', #3602, #5123 ) ;
#1640 = EDGE_CURVE ( 'NONE', #1805, #5526, #5135, .T. ) ;
#1641 = AXIS2_PLACEMENT_3D ( 'NONE', #5918, #4975, #566 ) ;
#1642 = DIRECTION ( 'NONE',  ( -0.000000000000000000, -0.000000000000000000, -1.000000000000000000 ) ) ;
#1643 = ORIENTED_EDGE ( 'NONE', *, *, #2188, .T. ) ;
#1644 = CARTESIAN_POINT ( 'NONE',  ( -14.34541152806172626, 17.98734769216428830, 2.761683449857409656 ) ) ;
#1645 = CARTESIAN_POINT ( 'NONE',  ( 7.460990961498263019, 21.75625611239105694, 30.97809455494030928 ) ) ;
#1646 = CIRCLE ( 'NONE', #422, 22.67164836619066648 ) ;
#1647 = EDGE_CURVE ( 'NONE', #4666, #2876, #3243, .T. ) ;
#1648 = CARTESIAN_POINT ( 'NONE',  ( 16.23652742703164975, 37.28747423195200383, -180.0000000000000000 ) ) ;
#1649 = AXIS2_PLACEMENT_3D ( 'NONE', #3095, #3187, #6033 ) ;
#1650 = PLANE ( 'NONE',  #1540 ) ;
#1651 = ORIENTED_EDGE ( 'NONE', *, *, #2390, .T. ) ;
#1652 = ORIENTED_EDGE ( 'NONE', *, *, #5237, .F. ) ;
#1653 = DIRECTION ( 'NONE',  ( 0.000000000000000000, -1.000000000000000000, 0.000000000000000000 ) ) ;
#1654 = EDGE_CURVE ( 'NONE', #5649, #2535, #2718, .T. ) ;
#1655 = VECTOR ( 'NONE', #1157, 1000.000000000000000 ) ;
#1656 = CARTESIAN_POINT ( 'NONE',  ( -20.00000000000000000, 0.000000000000000000, 51.00000000000002842 ) ) ;
#1657 = CARTESIAN_POINT ( 'NONE',  ( -43.99999999999990052, 13.41640786499905147, -65.00000000000000000 ) ) ;
#1658 = CARTESIAN_POINT ( 'NONE',  ( 8.000000000000007105, 72.93807001241029297, 0.000000000000000000 ) ) ;
#1659 = CIRCLE ( 'NONE', #954, 89.87058297576894006 ) ;
#1660 = FACE_OUTER_BOUND ( 'NONE', #2542, .T. ) ;
#1661 = ORIENTED_EDGE ( 'NONE', *, *, #1892, .T. ) ;
#1662 = FACE_OUTER_BOUND ( 'NONE', #6247, .T. ) ;
#1663 = ORIENTED_EDGE ( 'NONE', *, *, #660, .T. ) ;
#1664 = CARTESIAN_POINT ( 'NONE',  ( -3.061616997868383043E-15, -25.00000000000000000, -95.00000000000000000 ) ) ;
#1665 = ORIENTED_EDGE ( 'NONE', *, *, #3879, .F. ) ;
#1666 = CARTESIAN_POINT ( 'NONE',  ( 262.0000000000000000, 68.99999999999997158, 0.000000000000000000 ) ) ;
#1667 = ADVANCED_FACE ( 'NONE', ( #1582 ), #1164, .F. ) ;
#1668 = LINE ( 'NONE', #6090, #3986 ) ;
#1669 = DIRECTION ( 'NONE',  ( 1.000000000000000000, 0.000000000000000000, 0.000000000000000000 ) ) ;
#1670 = ORIENTED_EDGE ( 'NONE', *, *, #875, .F. ) ;
#1671 = SURFACE_STYLE_USAGE ( .BOTH. , #6093 ) ;
#1672 = CIRCLE ( 'NONE', #6103, 46.00000000000000000 ) ;
#1673 = CARTESIAN_POINT ( 'NONE',  ( 212.0000000000000284, 68.99999999999997158, 110.0000000000000000 ) ) ;
#1674 = CARTESIAN_POINT ( 'NONE',  ( -6.978968890507021960, 21.91580918028467195, 29.01915572147083822 ) ) ;
#1675 = CARTESIAN_POINT ( 'NONE',  ( -44.00000000000000000, -13.41640786499873172, -240.0000000000000000 ) ) ;
#1676 = CARTESIAN_POINT ( 'NONE',  ( 0.000000000000000000, 0.000000000000000000, -248.0000000000000000 ) ) ;
#1677 = ORIENTED_EDGE ( 'NONE', *, *, #5795, .T. ) ;
#1678 = EDGE_LOOP ( 'NONE', ( #4173, #1315, #5073, #3645 ) ) ;
#1679 = VERTEX_POINT ( 'NONE', #1560 ) ;
#1680 = CARTESIAN_POINT ( 'NONE',  ( 17.00000000000000000, 2.081899558550500280E-15, 48.00000000000000000 ) ) ;
#1681 = PRODUCT ( 'Part 32,1_Varsay\X2\0131\X0\lan', 'Part 32,1_Varsay\X2\0131\X0\lan', '', ( #5150 ) ) ;
#1682 = DIRECTION ( 'NONE',  ( 0.000000000000000000, 1.000000000000000000, -0.000000000000000000 ) ) ;
#1683 = DIRECTION ( 'NONE',  ( 0.000000000000000000, 0.000000000000000000, 1.000000000000000000 ) ) ;
#1684 = DIRECTION ( 'NONE',  ( 0.000000000000000000, -1.000000000000000000, 0.000000000000000000 ) ) ;
#1685 = CARTESIAN_POINT ( 'NONE',  ( -14.33006727100666033, -20.49285708348135415, 2.782958588747959983 ) ) ;
#1686 = EDGE_LOOP ( 'NONE', ( #27, #4335, #3100, #3984 ) ) ;
#1687 = SHAPE_REPRESENTATION ( 'Part 32,4_Varsay\X2\0131\X0\lan', ( #6349 ), #1927 ) ;
#1688 = DIRECTION ( 'NONE',  ( -0.000000000000000000, -0.000000000000000000, -1.000000000000000000 ) ) ;
#1689 = SHAPE_DEFINITION_REPRESENTATION ( #6167, #1687 ) ;
#1690 = CYLINDRICAL_SURFACE ( 'NONE', #2622, 17.00000000000000000 ) ;
#1691 = VERTEX_POINT ( 'NONE', #180 ) ;
#1692 = CARTESIAN_POINT ( 'NONE',  ( -6.500000000000005329, 120.0000000000000000, 16.00000000000000000 ) ) ;
#1693 = EDGE_LOOP ( 'NONE', ( #4587, #2710, #3591, #147 ) ) ;
#1694 = DIRECTION ( 'NONE',  ( -1.000000000000000000, 0.000000000000000000, 0.000000000000000000 ) ) ;
#1695 = AXIS2_PLACEMENT_3D ( 'NONE', #2603, #2512, #5997 ) ;
#1696 = CARTESIAN_POINT ( 'NONE',  ( 0.000000000000000000, 120.0000000000000000, 0.000000000000000000 ) ) ;
#1697 = CARTESIAN_POINT ( 'NONE',  ( 1.908796811648538206E-15, -20.00000000000000711, 39.27501000028011902 ) ) ;
#1698 = ORIENTED_EDGE ( 'NONE', *, *, #1630, .F. ) ;
#1699 = DIRECTION ( 'NONE',  ( 1.000000000000000000, 0.000000000000000000, 0.000000000000000000 ) ) ;
#1700 = SURFACE_SIDE_STYLE ('',( #2609 ) ) ;
#1701 = CARTESIAN_POINT ( 'NONE',  ( 0.000000000000000000, -17.00000000000000000, 5.000000000000004441 ) ) ;
#1702 = VECTOR ( 'NONE', #4647, 1000.000000000000000 ) ;
#1703 = DIRECTION ( 'NONE',  ( -0.000000000000000000, -0.000000000000000000, 1.000000000000000000 ) ) ;
#1704 = CARTESIAN_POINT ( 'NONE',  ( 0.000000000000000000, 120.0000000000000000, 12.00000000000000000 ) ) ;
#1705 = EDGE_CURVE ( 'NONE', #2388, #3408, #2321, .T. ) ;
#1706 = ORIENTED_EDGE ( 'NONE', *, *, #1918, .T. ) ;
#1707 = EDGE_CURVE ( 'NONE', #2247, #3626, #3138, .T. ) ;
#1708 = ORIENTED_EDGE ( 'NONE', *, *, #4886, .T. ) ;
#1709 = CARTESIAN_POINT ( 'NONE',  ( -1.231226070028328401, 24.97084192177787543, 39.17738101704807718 ) ) ;
#1710 = CIRCLE ( 'NONE', #4388, 4.000000000000003553 ) ;
#1711 = CARTESIAN_POINT ( 'NONE',  ( -16.23652742703190199, -37.28747423195189015, -160.0000000000000284 ) ) ;
#1712 = CARTESIAN_POINT ( 'NONE',  ( -16.23652742703189489, -37.28747423195188304, -110.0000000000000000 ) ) ;
#1713 = DIRECTION ( 'NONE',  ( 0.000000000000000000, 0.000000000000000000, -1.000000000000000000 ) ) ;
#1714 = ADVANCED_FACE ( 'NONE', ( #3040 ), #3073, .T. ) ;
#1715 = VECTOR ( 'NONE', #4781, 1000.000000000000000 ) ;
#1716 = ORIENTED_EDGE ( 'NONE', *, *, #5697, .T. ) ;
#1717 = CARTESIAN_POINT ( 'NONE',  ( -22.21770253897380343, -3.871672004622680241, -45.00000000000000000 ) ) ;
#1718 = ORIENTED_EDGE ( 'NONE', *, *, #4181, .F. ) ;
#1719 = AXIS2_PLACEMENT_3D ( 'NONE', #1717, #1238, #2004 ) ;
#1720 = DIRECTION ( 'NONE',  ( -0.000000000000000000, -0.000000000000000000, -1.000000000000000000 ) ) ;
#1721 = VECTOR ( 'NONE', #4989, 1000.000000000000000 ) ;
#1722 = EDGE_CURVE ( 'NONE', #1781, #5856, #149, .T. ) ;
#1723 = ITEM_DEFINED_TRANSFORMATION ( 'NONE', 'NONE', #3468,  #6349 ) ;
#1724 = CARTESIAN_POINT ( 'NONE',  ( -23.00000000000000000, 0.000000000000000000, 39.00000000000001421 ) ) ;
#1725 = PRODUCT_DEFINITION ( 'UNKNOWN', '', #4254, #5671 ) ;
#1726 = ORIENTED_EDGE ( 'NONE', *, *, #1194, .T. ) ;
#1727 = LINE ( 'NONE', #4691, #1545 ) ;
#1728 = ORIENTED_EDGE ( 'NONE', *, *, #4345, .F. ) ;
#1729 = ADVANCED_FACE ( 'NONE', ( #1133, #2166 ), #6042, .T. ) ;
#1730 = AXIS2_PLACEMENT_3D ( 'NONE', #5510, #5881, #3516 ) ;
#1731 = EDGE_CURVE ( 'NONE', #4627, #4783, #4864, .T. ) ;
#1732 = EDGE_CURVE ( 'NONE', #6264, #2677, #2102, .T. ) ;
#1733 = UNCERTAINTY_MEASURE_WITH_UNIT (LENGTH_MEASURE( 1.000000000000000082E-05 ), #3154, 'distance_accuracy_value', 'NONE');
#1734 = DIRECTION ( 'NONE',  ( 1.000000000000000000, 0.000000000000000000, 0.000000000000000000 ) ) ;
#1735 = VECTOR ( 'NONE', #687, 1000.000000000000000 ) ;
#1736 = CARTESIAN_POINT ( 'NONE',  ( 67.00000000000000000, 69.00000000000000000, 0.000000000000000000 ) ) ;
#1737 = UNCERTAINTY_MEASURE_WITH_UNIT (LENGTH_MEASURE( 1.000000000000000082E-05 ), #6051, 'distance_accuracy_value', 'NONE');
#1738 = DIRECTION ( 'NONE',  ( 1.000000000000000000, 0.000000000000000000, 0.000000000000000000 ) ) ;
#1739 = ORIENTED_EDGE ( 'NONE', *, *, #2123, .F. ) ;
#1740 = CARTESIAN_POINT ( 'NONE',  ( -12.81154844869972997, 19.11229287055882864, 4.578663348692236568 ) ) ;
#1742 = VERTEX_POINT ( 'NONE', #6102 ) ;
#1741 = AXIS2_PLACEMENT_3D ( 'NONE', #4620, #2682, #1713 ) ;
#1743 = AXIS2_PLACEMENT_3D ( 'NONE', #2403, #869, #5767 ) ;
#1744 = PRODUCT_DEFINITION_SHAPE ( 'NONE', 'NONE',  #2790 ) ;
#1745 = CARTESIAN_POINT ( 'NONE',  ( -43.99999999999990052, 13.41640786499905147, -49.99999999999999289 ) ) ;
#1746 = LINE ( 'NONE', #338, #2185 ) ;
#1747 = CIRCLE ( 'NONE', #1858, 17.00000000000000000 ) ;
#1748 = DIRECTION ( 'NONE',  ( -0.000000000000000000, -0.000000000000000000, 1.000000000000000000 ) ) ;
#1749 = CARTESIAN_POINT ( 'NONE',  ( 197.0000000000000000, 68.99999999999997158, 110.0000000000000000 ) ) ;
#1750 = EDGE_LOOP ( 'NONE', ( #789, #3524 ) ) ;
#1751 = ORIENTED_EDGE ( 'NONE', *, *, #1707, .F. ) ;
#1752 = AXIS2_PLACEMENT_3D ( 'NONE', #2533, #1415, #3508 ) ;
#1753 = CARTESIAN_POINT ( 'NONE',  ( -44.43364355155666345, 29.42304313293565343, -160.0000000000000284 ) ) ;
#1754 = AXIS2_PLACEMENT_3D ( 'NONE', #3517, #5484, #1066 ) ;
#1755 = FACE_OUTER_BOUND ( 'NONE', #3252, .T. ) ;
#1756 = CARTESIAN_POINT ( 'NONE',  ( 13.14183123006952947, -39.58265509608667543, -175.0000000000000284 ) ) ;
#1757 = DIRECTION ( 'NONE',  ( 1.000000000000000000, 0.000000000000000000, 0.000000000000000000 ) ) ;
#1758 = VERTEX_POINT ( 'NONE', #1680 ) ;
#1759 = DIRECTION ( 'NONE',  ( -0.000000000000000000, -0.000000000000000000, -1.000000000000000000 ) ) ;
#1760 = VERTEX_POINT ( 'NONE', #4056 ) ;
#1761=STYLED_ITEM('',(#6391),#151);
#1762 = PRESENTATION_LAYER_ASSIGNMENT (  '', '', ( #4631 ) ) ;
#1763 = DIRECTION ( 'NONE',  ( 1.000000000000000000, 0.000000000000000000, 0.000000000000000000 ) ) ;
#1764 = CARTESIAN_POINT ( 'NONE',  ( 15.23263781889692048, -17.24245498722747527, 1.434805278142651241 ) ) ;
#1765 = EDGE_LOOP ( 'NONE', ( #4569, #2233 ) ) ;
#1766 = DIRECTION ( 'NONE',  ( 0.000000000000000000, 1.000000000000000000, 0.000000000000000000 ) ) ;
#1767 = ORIENTED_EDGE ( 'NONE', *, *, #77, .F. ) ;
#1768 = VECTOR ( 'NONE', #1930, 1000.000000000000000 ) ;
#1769 = FACE_OUTER_BOUND ( 'NONE', #4542, .T. ) ;
#1770 = CARTESIAN_POINT ( 'NONE',  ( 0.000000000000000000, 0.000000000000000000, -248.0000000000000000 ) ) ;
#1771 = CARTESIAN_POINT ( 'NONE',  ( -22.21770253897380343, -3.871672004622680241, -180.0000000000000000 ) ) ;
#1772 = CARTESIAN_POINT ( 'NONE',  ( -7.451677332883843263, -23.86383568307784131, 30.79254100948602613 ) ) ;
#1773 = VERTEX_POINT ( 'NONE', #732 ) ;
#1774 = ORIENTED_EDGE ( 'NONE', *, *, #6177, .T. ) ;
#1775 = LINE ( 'NONE', #5265, #3301 ) ;
#1776 = CARTESIAN_POINT ( 'NONE',  ( 14.00000000000000000, 0.000000000000000000, 110.0000000000000000 ) ) ;
#1777 = LINE ( 'NONE', #5784, #5119 ) ;
#1778 = VECTOR ( 'NONE', #4640, 1000.000000000000000 ) ;
#1779 = CARTESIAN_POINT ( 'NONE',  ( 5.578949544899560742, -22.31500106593816213, 26.74243945601464745 ) ) ;
#1780 = ORIENTED_EDGE ( 'NONE', *, *, #776, .T. ) ;
#1781 = VERTEX_POINT ( 'NONE', #241 ) ;
#1782 = CARTESIAN_POINT ( 'NONE',  ( -5.133479616427195857, 24.46790356832289248, 26.30175839968468665 ) ) ;
#1783 = DIRECTION ( 'NONE',  ( 1.000000000000000000, 0.000000000000000000, 0.000000000000000000 ) ) ;
#1784 = DIRECTION ( 'NONE',  ( -0.000000000000000000, -0.000000000000000000, 1.000000000000000000 ) ) ;
#1785 = DIRECTION ( 'NONE',  ( -0.000000000000000000, 0.000000000000000000, 1.000000000000000000 ) ) ;
#1786 = VERTEX_POINT ( 'NONE', #5004 ) ;
#1787 = EDGE_LOOP ( 'NONE', ( #1631, #1107, #285, #744 ) ) ;
#1788 = ORIENTED_EDGE ( 'NONE', *, *, #100, .F. ) ;
#1789 = EDGE_CURVE ( 'NONE', #2013, #434, #1619, .T. ) ;
#1790 = DIRECTION ( 'NONE',  ( 1.000000000000000000, 0.000000000000000000, 0.000000000000000000 ) ) ;
#1791 = CONTEXT_DEPENDENT_SHAPE_REPRESENTATION ( #5011, #251 ) ;
#1792 = DIRECTION ( 'NONE',  ( 0.000000000000000000, 0.000000000000000000, 1.000000000000000000 ) ) ;
#1793 = CYLINDRICAL_SURFACE ( 'NONE', #722, 25.00000000000000000 ) ;
#1794 = PRODUCT_DEFINITION_FORMATION_WITH_SPECIFIED_SOURCE ( 'ANY', '', #657, .NOT_KNOWN. ) ;
#1795 = EDGE_LOOP ( 'NONE', ( #3572, #4949, #362, #4274 ) ) ;
#1796 = DIRECTION ( 'NONE',  ( -0.000000000000000000, -0.000000000000000000, -1.000000000000000000 ) ) ;
#1797 = ORIENTED_EDGE ( 'NONE', *, *, #1731, .T. ) ;
#1798 = ADVANCED_FACE ( 'NONE', ( #2833 ), #4766, .T. ) ;
#1799 = EDGE_CURVE ( 'NONE', #5724, #2249, #4712, .T. ) ;
#1800 = SURFACE_STYLE_USAGE ( .BOTH. , #6087 ) ;
#1801 = EDGE_CURVE ( 'NONE', #959, #2940, #3767, .T. ) ;
#1802 = DIRECTION ( 'NONE',  ( 0.000000000000000000, 0.000000000000000000, -1.000000000000000000 ) ) ;
#1803 = LINE ( 'NONE', #5776, #2531 ) ;
#1804 = DIRECTION ( 'NONE',  ( 0.000000000000000000, 0.000000000000000000, 1.000000000000000000 ) ) ;
#1805 = VERTEX_POINT ( 'NONE', #3195 ) ;
#1806 = ADVANCED_FACE ( 'NONE', ( #6164 ), #6201, .T. ) ;
#1807 = ADVANCED_FACE ( 'NONE', ( #1267 ), #3227, .T. ) ;
#1808 = CARTESIAN_POINT ( 'NONE',  ( 67.00000000000000000, 69.00000000000000000, 110.0000000000000000 ) ) ;
#1809 = ORIENTED_EDGE ( 'NONE', *, *, #2656, .T. ) ;
#1810 = CARTESIAN_POINT ( 'NONE',  ( -1.353091841878392376, 19.95700839110197933, 39.15972426387312311 ) ) ;
#1811 = LINE ( 'NONE', #1224, #3738 ) ;
#1812 = CIRCLE ( 'NONE', #3451, 12.50000000000001421 ) ;
#1813 = AXIS2_PLACEMENT_3D ( 'NONE', #5014, #616, #1174 ) ;
#1814 = CARTESIAN_POINT ( 'NONE',  ( -17.05141243254543681, -24.25762350764758679, 12.00000000000000000 ) ) ;
#1815 = CARTESIAN_POINT ( 'NONE',  ( 7.491878387983184062, -21.74571065617575982, 31.20484628725278498 ) ) ;
#1816 = VERTEX_POINT ( 'NONE', #4971 ) ;
#1817 = EDGE_CURVE ( 'NONE', #4938, #4122, #2289, .T. ) ;
#1818 = ORIENTED_EDGE ( 'NONE', *, *, #4397, .F. ) ;
#1819 = DIRECTION ( 'NONE',  ( -0.000000000000000000, -0.000000000000000000, -1.000000000000000000 ) ) ;
#1820 = CIRCLE ( 'NONE', #5111, 166.8359700257217071 ) ;
#1821 = CARTESIAN_POINT ( 'NONE',  ( 8.000000000000007105, 72.93807001241029297, 1.999999999999996669 ) ) ;
#1822 = LINE ( 'NONE', #345, #5035 ) ;
#1823 = PLANE ( 'NONE',  #415 ) ;
#1824 = ORIENTED_EDGE ( 'NONE', *, *, #6358, .F. ) ;
#1825 = ORIENTED_EDGE ( 'NONE', *, *, #3218, .T. ) ;
#1826 = PLANE ( 'NONE',  #4950 ) ;
#1827 = CARTESIAN_POINT ( 'NONE',  ( -13.41482486054669820, 26.39531364385071299, 6.264720534548226638 ) ) ;
#1828 = ORIENTED_EDGE ( 'NONE', *, *, #5315, .F. ) ;
#1829 = ADVANCED_FACE ( 'NONE', ( #14 ), #2930, .F. ) ;
#1830 = LINE ( 'NONE', #6183, #5979 ) ;
#1831 = EDGE_LOOP ( 'NONE', ( #6351, #5689, #2614, #5375 ) ) ;
#1832 = AXIS2_PLACEMENT_3D ( 'NONE', #1262, #2860, #852 ) ;
#1833 = DIRECTION ( 'NONE',  ( 1.000000000000000000, 0.000000000000000000, -0.000000000000000000 ) ) ;
#1834 = EDGE_CURVE ( 'NONE', #5091, #633, #4846, .T. ) ;
#1835 = CARTESIAN_POINT ( 'NONE',  ( -63.68819482895219153, 63.50744305896495234, 131.1935513772751847 ) ) ;
#1836 = CARTESIAN_POINT ( 'NONE',  ( 0.000000000000000000, 0.000000000000000000, 41.00000000000000000 ) ) ;
#1837 = CARTESIAN_POINT ( 'NONE',  ( 0.000000000000000000, 0.000000000000000000, -49.99999999999999289 ) ) ;
#1838 = AXIS2_PLACEMENT_3D ( 'NONE', #87, #4586, #4492 ) ;
#1839 = CARTESIAN_POINT ( 'NONE',  ( -5.641746473127986938, -24.35561814371765266, 36.72278580929200587 ) ) ;
#1840 = ORIENTED_EDGE ( 'NONE', *, *, #5629, .T. ) ;
#1841 = CARTESIAN_POINT ( 'NONE',  ( 265.0000000000000000, 0.000000000000000000, 110.0000000000000000 ) ) ;
#1842 = CARTESIAN_POINT ( 'NONE',  ( 5.475713916123539526, 24.39360375241167134, 36.90593746307732204 ) ) ;
#1843 = CARTESIAN_POINT ( 'NONE',  ( -44.64065620456893413, -28.99954194078699032, -180.0000000000000000 ) ) ;
#1844 = CIRCLE ( 'NONE', #3580, 25.00000000000000000 ) ;
#1845 = ADVANCED_FACE ( 'NONE', ( #1521 ), #3907, .T. ) ;
#1846 = DIRECTION ( 'NONE',  ( 1.000000000000000000, 0.000000000000000000, 0.000000000000000000 ) ) ;
#1847 = CARTESIAN_POINT ( 'NONE',  ( 2.421623179306582330, -24.88356973210974843, 24.67241923065279607 ) ) ;
#1848 = ORIENTED_EDGE ( 'NONE', *, *, #3527, .T. ) ;
#1849 = VECTOR ( 'NONE', #153, 1000.000000000000000 ) ;
#1850 = AXIS2_PLACEMENT_3D ( 'NONE', #2052, #4012, #4652 ) ;
#1851 = ORIENTED_EDGE ( 'NONE', *, *, #3532, .F. ) ;
#1852 =( REPRESENTATION_RELATIONSHIP ('NONE','NONE', #632, #3711 ) REPRESENTATION_RELATIONSHIP_WITH_TRANSFORMATION ( #5727 )SHAPE_REPRESENTATION_RELATIONSHIP( ) );
#1853 = CARTESIAN_POINT ( 'NONE',  ( -6.367429986337528547, 24.17592611763979704, 35.74554154416229323 ) ) ;
#1854 = AXIS2_PLACEMENT_3D ( 'NONE', #2040, #1556, #599 ) ;
#1855 = DIRECTION ( 'NONE',  ( 1.000000000000000000, 0.000000000000000000, 0.000000000000000000 ) ) ;
#1856 = LINE ( 'NONE', #1393, #4206 ) ;
#1857 = DIRECTION ( 'NONE',  ( -0.000000000000000000, -0.000000000000000000, -1.000000000000000000 ) ) ;
#1858 = AXIS2_PLACEMENT_3D ( 'NONE', #4991, #2417, #4935 ) ;
#1859 = EDGE_LOOP ( 'NONE', ( #4915, #6008, #2084, #3850 ) ) ;
#1860 = ORIENTED_EDGE ( 'NONE', *, *, #1060, .F. ) ;
#1861 = B_SPLINE_CURVE_WITH_KNOTS ( 'NONE', 3,
 ( #5961, #92, #2624, #4066 ),
 .UNSPECIFIED., .F., .F.,
 ( 4, 4 ),
 ( 0.000000000000000000, 0.002032958594636734458 ),
 .UNSPECIFIED. ) ;
#1862 = CARTESIAN_POINT ( 'NONE',  ( 0.2052511266213280505, 21.25619793154159964, -225.0000000000000000 ) ) ;
#1863 = AXIS2_PLACEMENT_3D ( 'NONE', #1664, #2601, #4628 ) ;
#1864 = CARTESIAN_POINT ( 'NONE',  ( -12.54049055679406344, 29.87738611749458428, 9.974675204776749737 ) ) ;
#1865 = AXIS2_PLACEMENT_3D ( 'NONE', #991, #3824, #3397 ) ;
#1866 = DIRECTION ( 'NONE',  ( -0.000000000000000000, -0.000000000000000000, -1.000000000000000000 ) ) ;
#1867 = ORIENTED_EDGE ( 'NONE', *, *, #4266, .T. ) ;
#1868 = ORIENTED_EDGE ( 'NONE', *, *, #5232, .T. ) ;
#1869 = LINE ( 'NONE', #1349, #2329 ) ;
#1870 =( NAMED_UNIT ( * ) PLANE_ANGLE_UNIT ( ) SI_UNIT ( $, .RADIAN. ) );
#1871 = DIRECTION ( 'NONE',  ( 0.000000000000000000, 0.000000000000000000, -1.000000000000000000 ) ) ;
#1872 = FACE_OUTER_BOUND ( 'NONE', #4882, .T. ) ;
#1873 = CARTESIAN_POINT ( 'NONE',  ( -6.097143767825691008, -24.24550159253069026, 36.14924867743861370 ) ) ;
#1874 = ORIENTED_EDGE ( 'NONE', *, *, #2934, .F. ) ;
#1875 = DIRECTION ( 'NONE',  ( -1.000000000000000000, 0.000000000000000000, 0.000000000000000000 ) ) ;
#1876 = CARTESIAN_POINT ( 'NONE',  ( -17.00000000000000000, 2.081899558550500280E-15, -45.00000000000000000 ) ) ;
#1877 = CARTESIAN_POINT ( 'NONE',  ( 25.00000000000000000, 0.000000000000000000, 0.000000000000000000 ) ) ;
#1878 = ADVANCED_FACE ( 'NONE', ( #4424 ), #5915, .F. ) ;
#1879 = CARTESIAN_POINT ( 'NONE',  ( -43.99999999999990052, 13.41640786499905147, -160.0000000000000284 ) ) ;
#1880 = CARTESIAN_POINT ( 'NONE',  ( 6.724622458085284471, -24.07890901287614227, 35.10508533856562252 ) ) ;
#1881 = VERTEX_POINT ( 'NONE', #2006 ) ;
#1882 = DIRECTION ( 'NONE',  ( 0.000000000000000000, 0.000000000000000000, -1.000000000000000000 ) ) ;
#1883 = ORIENTED_EDGE ( 'NONE', *, *, #6026, .T. ) ;
#1884 = DIRECTION ( 'NONE',  ( -0.000000000000000000, -0.000000000000000000, -1.000000000000000000 ) ) ;
#1885 = ADVANCED_FACE ( 'NONE', ( #3452 ), #2392, .F. ) ;
#1886 = LINE ( 'NONE', #5301, #5789 ) ;
#1887 = LINE ( 'NONE', #827, #1418 ) ;
#1888 = CYLINDRICAL_SURFACE ( 'NONE', #3173, 166.8359700257217071 ) ;
#1889 = ORIENTED_EDGE ( 'NONE', *, *, #2548, .T. ) ;
#1890 = ORIENTED_EDGE ( 'NONE', *, *, #5812, .T. ) ;
#1891 = ADVANCED_FACE ( 'NONE', ( #5425, #3488 ), #5883, .T. ) ;
#1892 = EDGE_CURVE ( 'NONE', #1339, #5491, #36, .T. ) ;
#1893 = CARTESIAN_POINT ( 'NONE',  ( 174.7835321302054865, 68.75545066608756883, 9.999999999999996447 ) ) ;
#1894 = CARTESIAN_POINT ( 'NONE',  ( -12.47915588485122917, 30.13418267071338263, 9.999999999999991118 ) ) ;
#1895 = CARTESIAN_POINT ( 'NONE',  ( 12.78450670028659886, -21.48642263404485320, 4.587769495204018888 ) ) ;
#1896 = VERTEX_POINT ( 'NONE', #3388 ) ;
#1897 = DIRECTION ( 'NONE',  ( 1.000000000000000000, 0.000000000000000000, 0.000000000000000000 ) ) ;
#1898 = CARTESIAN_POINT ( 'NONE',  ( -7.481756639719942648, -21.74910199390652465, 31.20551891105749931 ) ) ;
#1899 = CARTESIAN_POINT ( 'NONE',  ( -17.00000000000000000, 25.00000000000000000, -195.0000000000000000 ) ) ;
#1900 = CARTESIAN_POINT ( 'NONE',  ( -0.9839074788235784297, -24.98539006426129561, 39.22674605012092997 ) ) ;
#1901 = ORIENTED_EDGE ( 'NONE', *, *, #6210, .F. ) ;
#1902 = CARTESIAN_POINT ( 'NONE',  ( -19.00000000000000000, 2.326828918379970970E-15, -240.0000000000000000 ) ) ;
#1903 = DIRECTION ( 'NONE',  ( 0.000000000000000000, 0.000000000000000000, 1.000000000000000000 ) ) ;
#1904 = CARTESIAN_POINT ( 'NONE',  ( 17.00000000000000000, 25.00000000000000000, -30.00000000000000000 ) ) ;
#1905 = CARTESIAN_POINT ( 'NONE',  ( 6.367429986337532988, -24.17592611763979704, 35.74554154416227192 ) ) ;
#1906 = VERTEX_POINT ( 'NONE', #2901 ) ;
#1907 = ADVANCED_FACE ( 'NONE', ( #4452 ), #6327, .T. ) ;
#1908 = DIRECTION ( 'NONE',  ( -0.000000000000000000, -0.000000000000000000, -1.000000000000000000 ) ) ;
#1909 = ORIENTED_EDGE ( 'NONE', *, *, #5738, .F. ) ;
#1910 = CARTESIAN_POINT ( 'NONE',  ( -6.135028333862784677, 22.16704433745741554, 36.09490741883096376 ) ) ;
#1911 = EDGE_CURVE ( 'NONE', #2192, #4936, #2298, .T. ) ;
#1912 = DIRECTION ( 'NONE',  ( -0.000000000000000000, -0.000000000000000000, -1.000000000000000000 ) ) ;
#1913 = EDGE_CURVE ( 'NONE', #4936, #635, #6073, .T. ) ;
#1914 = DIRECTION ( 'NONE',  ( 1.000000000000000000, 0.000000000000000000, 0.000000000000000000 ) ) ;
#1915 = CARTESIAN_POINT ( 'NONE',  ( 44.00000000000008527, 13.41640786499836224, -49.99999999999999289 ) ) ;
#1916 = ORIENTED_EDGE ( 'NONE', *, *, #5904, .F. ) ;
#1917 = ORIENTED_EDGE ( 'NONE', *, *, #4670, .F. ) ;
#1918 = EDGE_CURVE ( 'NONE', #4195, #3357, #1359, .T. ) ;
#1919 = CARTESIAN_POINT ( 'NONE',  ( 22.00000000000000000, 2.694222958124176809E-15, 44.00000000000000711 ) ) ;
#1920 = CIRCLE ( 'NONE', #6040, 72.49991987048069575 ) ;
#1921 = DIRECTION ( 'NONE',  ( 1.000000000000000000, 0.000000000000000000, 0.000000000000000000 ) ) ;
#1922 = EDGE_CURVE ( 'NONE', #1071, #4348, #1672, .T. ) ;
#1923 = CIRCLE ( 'NONE', #4500, 17.00000000000000000 ) ;
#1924 = DIRECTION ( 'NONE',  ( 0.000000000000000000, 0.000000000000000000, 1.000000000000000000 ) ) ;
#1925 = ORIENTED_EDGE ( 'NONE', *, *, #2923, .T. ) ;
#1926 = ADVANCED_FACE ( 'NONE', ( #6156 ), #2672, .T. ) ;
#1927 =( GEOMETRIC_REPRESENTATION_CONTEXT ( 3 ) GLOBAL_UNCERTAINTY_ASSIGNED_CONTEXT ( ( #2692 ) ) GLOBAL_UNIT_ASSIGNED_CONTEXT ( ( #5255, #3769, #1213 ) ) REPRESENTATION_CONTEXT ( 'NONE', 'WORKASPACE' ) );
#1928 = PRODUCT_DEFINITION ( 'UNKNOWN', '', #1794, #1467 ) ;
#1929 = DIRECTION ( 'NONE',  ( -1.687281020732334463E-17, 0.6322580582614716338, -0.7747578639571421899 ) ) ;
#1930 = DIRECTION ( 'NONE',  ( 0.000000000000000000, 1.000000000000000000, -0.000000000000000000 ) ) ;
#1931 = CARTESIAN_POINT ( 'NONE',  ( 0.000000000000000000, 0.000000000000000000, 110.0000000000000000 ) ) ;
#1932 =( REPRESENTATION_RELATIONSHIP ('NONE','NONE', #632, #5606 ) REPRESENTATION_RELATIONSHIP_WITH_TRANSFORMATION ( #5349 )SHAPE_REPRESENTATION_RELATIONSHIP( ) );
#1933 = DIRECTION ( 'NONE',  ( 1.000000000000000000, 0.000000000000000000, 0.000000000000000000 ) ) ;
#1934 = ORIENTED_EDGE ( 'NONE', *, *, #4837, .F. ) ;
#1935 = FACE_OUTER_BOUND ( 'NONE', #2276, .T. ) ;
#1936 = AXIS2_PLACEMENT_3D ( 'NONE', #4281, #3808, #5196 ) ;
#1937 = EDGE_CURVE ( 'NONE', #5271, #117, #4669, .T. ) ;
#1938 = CARTESIAN_POINT ( 'NONE',  ( -17.05141243254543681, 0.000000000000000000, 12.00000000000000000 ) ) ;
#1939 = DIRECTION ( 'NONE',  ( 1.000000000000000000, 0.000000000000000000, -0.000000000000000000 ) ) ;
#1940 = AXIS2_PLACEMENT_3D ( 'NONE', #3842, #2866, #4349 ) ;
#1941 = CARTESIAN_POINT ( 'NONE',  ( -0.000000000000000000, 76.99999716619419132, 0.000000000000000000 ) ) ;
#1942 = DIRECTION ( 'NONE',  ( 1.000000000000000000, 0.000000000000000000, 0.000000000000000000 ) ) ;
#1943 = ORIENTED_EDGE ( 'NONE', *, *, #3209, .F. ) ;
#1944 = CARTESIAN_POINT ( 'NONE',  ( 23.00000000000000000, 2.816687638038912352E-15, 39.00000000000001421 ) ) ;
#1945 = AXIS2_PLACEMENT_3D ( 'NONE', #4470, #5478, #2920 ) ;
#1946 = LINE ( 'NONE', #3387, #630 ) ;
#1947 = DIRECTION ( 'NONE',  ( -0.000000000000000000, -0.000000000000000000, 1.000000000000000000 ) ) ;
#1948 = DIRECTION ( 'NONE',  ( 1.000000000000000000, 0.000000000000000000, 0.000000000000000000 ) ) ;
#1949 = CARTESIAN_POINT ( 'NONE',  ( -3.081487911019577365E-30, 5.660601460262082306E-46, 281.0000000000000000 ) ) ;
#1950 = CIRCLE ( 'NONE', #822, 90.00000000000000000 ) ;
#1951 = DIRECTION ( 'NONE',  ( -0.000000000000000000, -0.000000000000000000, 1.000000000000000000 ) ) ;
#1952 = ORIENTED_EDGE ( 'NONE', *, *, #1411, .F. ) ;
#1953 = VERTEX_POINT ( 'NONE', #2765 ) ;
#1954 = ORIENTED_EDGE ( 'NONE', *, *, #3238, .F. ) ;
#1955 = EDGE_LOOP ( 'NONE', ( #3744, #550, #5018, #3634 ) ) ;
#1956 = FACE_OUTER_BOUND ( 'NONE', #872, .T. ) ;
#1957 = DIRECTION ( 'NONE',  ( -0.000000000000000000, 0.000000000000000000, -1.000000000000000000 ) ) ;
#1958 = CIRCLE ( 'NONE', #2667, 89.87058297576894006 ) ;
#1959 = LINE ( 'NONE', #2405, #6056 ) ;
#1960 = ORIENTED_EDGE ( 'NONE', *, *, #322, .F. ) ;
#1961 = AXIS2_PLACEMENT_3D ( 'NONE', #4960, #4467, #5387 ) ;
#1962 = DIRECTION ( 'NONE',  ( -0.000000000000000000, -0.000000000000000000, -1.000000000000000000 ) ) ;
#1963 = CARTESIAN_POINT ( 'NONE',  ( -6.802364521716127044, -21.97126452515143313, 28.60827024242000149 ) ) ;
#1964 = CIRCLE ( 'NONE', #1754, 90.00000000000319744 ) ;
#1965 = PLANE ( 'NONE',  #3668 ) ;
#1966 = CARTESIAN_POINT ( 'NONE',  ( 0.000000000000000000, 25.00000000000000000, -20.00000000000000000 ) ) ;
#1967 = ORIENTED_EDGE ( 'NONE', *, *, #2075, .T. ) ;
#1968 = FACE_OUTER_BOUND ( 'NONE', #2369, .T. ) ;
#1969 = ORIENTED_EDGE ( 'NONE', *, *, #2109, .F. ) ;
#1970 = EDGE_CURVE ( 'NONE', #6010, #3220, #6258, .T. ) ;
#1971 = CIRCLE ( 'NONE', #4743, 6.500000000000005329 ) ;
#1972 = FACE_OUTER_BOUND ( 'NONE', #4062, .T. ) ;
#1973 = CARTESIAN_POINT ( 'NONE',  ( 0.4985038669289038604, 25.00000000000000000, 24.27501000028010480 ) ) ;
#1974 = CARTESIAN_POINT ( 'NONE',  ( -13.41482486054668044, 26.39531364385071299, 5.999999999999990230 ) ) ;
#1975 = AXIS2_PLACEMENT_3D ( 'NONE', #5093, #3455, #6119 ) ;
#1976 = DIRECTION ( 'NONE',  ( 0.000000000000000000, 0.000000000000000000, -1.000000000000000000 ) ) ;
#1977 = ORIENTED_EDGE ( 'NONE', *, *, #4314, .T. ) ;
#1978 = CARTESIAN_POINT ( 'NONE',  ( 3.536994606882255532, 22.74309932279132340, 9.666805580179055113 ) ) ;
#1979 = ORIENTED_EDGE ( 'NONE', *, *, #2532, .F. ) ;
#1980 = CARTESIAN_POINT ( 'NONE',  ( 0.000000000000000000, 76.99999716619419132, 281.0000000000000000 ) ) ;
#1981 = DIRECTION ( 'NONE',  ( 0.000000000000000000, 0.000000000000000000, 1.000000000000000000 ) ) ;
#1982 = PLANE ( 'NONE',  #4918 ) ;
#1983 = CARTESIAN_POINT ( 'NONE',  ( -15.99408614349810698, 25.00000000000000000, -4.336808689942017736E-15 ) ) ;
#1984 = ORIENTED_EDGE ( 'NONE', *, *, #2469, .T. ) ;
#1985 = ORIENTED_EDGE ( 'NONE', *, *, #23, .F. ) ;
#1986 = ORIENTED_EDGE ( 'NONE', *, *, #2769, .F. ) ;
#1987 = CARTESIAN_POINT ( 'NONE',  ( 13.27343467285273171, 26.93736435430922072, 3.972397629097673022 ) ) ;
#1988 = CARTESIAN_POINT ( 'NONE',  ( 16.00000000000000355, 1.959434878635765526E-15, -4.000000000000000000 ) ) ;
#1989 = AXIS2_PLACEMENT_3D ( 'NONE', #5106, #697, #4615 ) ;
#1990 = CARTESIAN_POINT ( 'NONE',  ( 11.91160812950988124, -21.98255961136171877, 5.429893957167271523 ) ) ;
#1991 = ORIENTED_EDGE ( 'NONE', *, *, #473, .F. ) ;
#1992 = CARTESIAN_POINT ( 'NONE',  ( -33.68819482895218442, 82.87638965790608836, 249.6200851762759498 ) ) ;
#1993 = DIRECTION ( 'NONE',  ( -0.000000000000000000, -0.000000000000000000, 1.000000000000000000 ) ) ;
#1994 = PLANE ( 'NONE',  #1344 ) ;
#1995 = VERTEX_POINT ( 'NONE', #4740 ) ;
#1996 = EDGE_CURVE ( 'NONE', #1896, #1020, #1811, .T. ) ;
#1997 = VERTEX_POINT ( 'NONE', #1701 ) ;
#1998 = FACE_OUTER_BOUND ( 'NONE', #4911, .T. ) ;
#1999 = DIRECTION ( 'NONE',  ( -0.000000000000000000, 0.000000000000000000, -1.000000000000000000 ) ) ;
#2000 = EDGE_CURVE ( 'NONE', #2906, #3955, #6208, .T. ) ;
#2001 = CARTESIAN_POINT ( 'NONE',  ( 0.000000000000000000, 0.000000000000000000, 0.000000000000000000 ) ) ;
#2002 = LINE ( 'NONE', #497, #2363 ) ;
#2003 = ORIENTED_EDGE ( 'NONE', *, *, #6291, .F. ) ;
#2004 = DIRECTION ( 'NONE',  ( 1.000000000000000000, 0.000000000000000000, -0.000000000000000000 ) ) ;
#2005 = ORIENTED_EDGE ( 'NONE', *, *, #3343, .F. ) ;
#2006 = CARTESIAN_POINT ( 'NONE',  ( -44.00000000000000000, -13.41640786499873172, 15.00000000000000000 ) ) ;
#2007 = LINE ( 'NONE', #5916, #5573 ) ;
#2008 = PRODUCT_DEFINITION ( 'UNKNOWN', '', #4145, #5528 ) ;
#2009 = CARTESIAN_POINT ( 'NONE',  ( 19.00000000000000000, 2.326828918379970970E-15, 23.00000000000000000 ) ) ;
#2010 = CARTESIAN_POINT ( 'NONE',  ( 0.000000000000000000, 0.000000000000000000, 281.0000000000000000 ) ) ;
#2011 = EDGE_CURVE ( 'NONE', #6264, #336, #1746, .T. ) ;
#2012 = ORIENTED_EDGE ( 'NONE', *, *, #4103, .T. ) ;
#2013 = VERTEX_POINT ( 'NONE', #2187 ) ;
#2014 = ORIENTED_EDGE ( 'NONE', *, *, #5278, .F. ) ;
#2015 = LINE ( 'NONE', #54, #5517 ) ;
#2016 = AXIS2_PLACEMENT_3D ( 'NONE', #3442, #428, #2384 ) ;
#2017 = CARTESIAN_POINT ( 'NONE',  ( -2.385244779468109755E-15, -1.040834085586084257E-14, -115.0000000000000000 ) ) ;
#2018 = AXIS2_PLACEMENT_3D ( 'NONE', #5052, #4496, #3110 ) ;
#2019 = CARTESIAN_POINT ( 'NONE',  ( 0.000000000000000000, 0.000000000000000000, 47.00000000000000000 ) ) ;
#2020 = ORIENTED_EDGE ( 'NONE', *, *, #4201, .T. ) ;
#2021 = AXIS2_PLACEMENT_3D ( 'NONE', #1334, #3871, #4847 ) ;
#2022 = VECTOR ( 'NONE', #2820, 1000.000000000000000 ) ;
#2023 = CARTESIAN_POINT ( 'NONE',  ( -44.64065620456596406, -28.99954194078535963, -225.0000000000000000 ) ) ;
#2024 = CARTESIAN_POINT ( 'NONE',  ( -0.2052511266214760433, -21.25619793154163517, -49.99999999999999289 ) ) ;
#2025 = AXIS2_PLACEMENT_3D ( 'NONE', #3027, #3988, #5969 ) ;
#2026 = DIRECTION ( 'NONE',  ( -0.000000000000000000, -0.000000000000000000, -1.000000000000000000 ) ) ;
#2027 = VERTEX_POINT ( 'NONE', #4144 ) ;
#2028 = PLANE ( 'NONE',  #3585 ) ;
#2029 = EDGE_LOOP ( 'NONE', ( #481, #706, #440, #1979, #1751, #4429 ) ) ;
#2030 = CARTESIAN_POINT ( 'NONE',  ( 0.000000000000000000, 17.00000000000000000, 276.0000000000000000 ) ) ;
#2031 = CARTESIAN_POINT ( 'NONE',  ( 107.0000000000000142, 69.00000000000000000, 110.0000000000000000 ) ) ;
#2032 = CIRCLE ( 'NONE', #4494, 19.00000000000000000 ) ;
#2033 = CARTESIAN_POINT ( 'NONE',  ( 1.231226070028332398, -24.97084192177786832, 39.17738101704806297 ) ) ;
#2034 = VERTEX_POINT ( 'NONE', #262 ) ;
#2035 = DIRECTION ( 'NONE',  ( 0.000000000000000000, -1.000000000000000000, -1.247733429937938623E-16 ) ) ;
#2036 = VERTEX_POINT ( 'NONE', #757 ) ;
#2037 = CARTESIAN_POINT ( 'NONE',  ( -5.269070065585171214, 22.39093555978999817, 26.41927588677976502 ) ) ;
#2038 = AXIS2_PLACEMENT_3D ( 'NONE', #2001, #3381, #586 ) ;
#2039 = CARTESIAN_POINT ( 'NONE',  ( -22.00000000000000000, 0.000000000000000000, 44.00000000000000711 ) ) ;
#2040 = CARTESIAN_POINT ( 'NONE',  ( 0.000000000000000000, 0.000000000000000000, 50.00000000000000711 ) ) ;
#2041 = TOROIDAL_SURFACE ( 'NONE', #2446, 6.500000000000000000, 1.000000000000000000 ) ;
#2042 = EDGE_LOOP ( 'NONE', ( #5382, #6214 ) ) ;
#2043 = ORIENTED_EDGE ( 'NONE', *, *, #315, .T. ) ;
#2044 = ORIENTED_EDGE ( 'NONE', *, *, #1118, .T. ) ;
#2045 = COLOUR_RGB ( '',0.7921568627450980005, 0.8196078431372548767, 0.9333333333333333481 ) ;
#2046 = CARTESIAN_POINT ( 'NONE',  ( 44.00000000000008527, 13.41640786499836224, -160.0000000000000284 ) ) ;
#2047 = CARTESIAN_POINT ( 'NONE',  ( 20.00000000000000000, 2.449293598294706513E-15, 51.00000000000002842 ) ) ;
#2048 = AXIS2_PLACEMENT_3D ( 'NONE', #3818, #5792, #4257 ) ;
#2049 = CYLINDRICAL_SURFACE ( 'NONE', #5959, 90.00000000000318323 ) ;
#2050 = VERTEX_POINT ( 'NONE', #1320 ) ;
#2051 = AXIS2_PLACEMENT_3D ( 'NONE', #4987, #1003, #3477 ) ;
#2052 = CARTESIAN_POINT ( 'NONE',  ( 0.000000000000000000, 0.000000000000000000, -110.0000000000000000 ) ) ;
#2053 = AXIS2_PLACEMENT_3D ( 'NONE', #3009, #2457, #18 ) ;
#2054 =( NAMED_UNIT ( * ) PLANE_ANGLE_UNIT ( ) SI_UNIT ( $, .RADIAN. ) );
#2055 = CARTESIAN_POINT ( 'NONE',  ( -5.735021534702854140, -22.27575375288411408, 36.62858606677772144 ) ) ;
#2056 = DIRECTION ( 'NONE',  ( -0.000000000000000000, -0.000000000000000000, -1.000000000000000000 ) ) ;
#2057 = ORIENTED_EDGE ( 'NONE', *, *, #4660, .T. ) ;
#2058 = VECTOR ( 'NONE', #2660, 1000.000000000000000 ) ;
#2059 = CARTESIAN_POINT ( 'NONE',  ( 0.000000000000000000, 0.000000000000000000, 1.000000000000000888 ) ) ;
#2060 = CIRCLE ( 'NONE', #2160, 24.99999999999999289 ) ;
#2061 = AXIS2_PLACEMENT_3D ( 'NONE', #4763, #1347, #355 ) ;
#2062 = DIRECTION ( 'NONE',  ( -0.000000000000000000, -0.000000000000000000, -1.000000000000000000 ) ) ;
#2063 = CARTESIAN_POINT ( 'NONE',  ( 15.99408614349810698, 19.21429697996681796, 0.000000000000000000 ) ) ;
#2064 = ORIENTED_EDGE ( 'NONE', *, *, #1058, .F. ) ;
#2065 = AXIS2_PLACEMENT_3D ( 'NONE', #1893, #3851, #3360 ) ;
#2066 = FILL_AREA_STYLE_COLOUR ( '', #2234 ) ;
#2067 = DIRECTION ( 'NONE',  ( 0.000000000000000000, 1.000000000000000000, 0.000000000000000000 ) ) ;
#2068 = CARTESIAN_POINT ( 'NONE',  ( 0.4497881292104084494, 22.99670767401471849, 24.28508774596658526 ) ) ;
#2069 = DIRECTION ( 'NONE',  ( 1.000000000000000000, 0.000000000000000000, 0.000000000000000000 ) ) ;
#2070 = CYLINDRICAL_SURFACE ( 'NONE', #5040, 19.00000000000000000 ) ;
#2071 = EDGE_LOOP ( 'NONE', ( #5252, #891, #5516, #128 ) ) ;
#2072 = ORIENTED_EDGE ( 'NONE', *, *, #2303, .T. ) ;
#2073 = ORIENTED_EDGE ( 'NONE', *, *, #1654, .F. ) ;
#2074 = VECTOR ( 'NONE', #874, 1000.000000000000000 ) ;
#2075 = EDGE_CURVE ( 'NONE', #4556, #4140, #4342, .T. ) ;
#2076 = CYLINDRICAL_SURFACE ( 'NONE', #4374, 4.000000000000000000 ) ;
#2077 = EDGE_CURVE ( 'NONE', #1953, #1273, #2903, .T. ) ;
#2078 = DIRECTION ( 'NONE',  ( 1.000000000000000000, 0.000000000000000000, 0.000000000000000000 ) ) ;
#2079 = DIRECTION ( 'NONE',  ( 1.000000000000000000, 0.000000000000000000, 0.000000000000000000 ) ) ;
#2080 = CARTESIAN_POINT ( 'NONE',  ( -3.081487911019577365E-30, 5.660601460262082306E-46, 281.0000000000000000 ) ) ;
#2081 = EDGE_CURVE ( 'NONE', #4602, #3869, #141, .T. ) ;
#2082 = EDGE_CURVE ( 'NONE', #2034, #1488, #4773, .T. ) ;
#2083 = DIRECTION ( 'NONE',  ( -0.000000000000000000, 0.000000000000000000, 1.000000000000000000 ) ) ;
#2084 = ORIENTED_EDGE ( 'NONE', *, *, #2349, .F. ) ;
#2085 = DIRECTION ( 'NONE',  ( 4.170590109825017016E-16, -0.0002856477006241188183, 0.9999999592026946882 ) ) ;
#2086 = CARTESIAN_POINT ( 'NONE',  ( -3.680439676527237136, -22.70725644061459647, 38.32515107347151684 ) ) ;
#2087 = AXIS2_PLACEMENT_3D ( 'NONE', #1753, #3719, #5683 ) ;
#2088 = CYLINDRICAL_SURFACE ( 'NONE', #1863, 17.00000000000000000 ) ;
#2089 = ORIENTED_EDGE ( 'NONE', *, *, #1611, .T. ) ;
#2090 = DIRECTION ( 'NONE',  ( -1.000000000000000000, 0.000000000000000000, 0.000000000000000000 ) ) ;
#2091 = CARTESIAN_POINT ( 'NONE',  ( 0.000000000000000000, 76.99999716619419132, 276.0000000000000000 ) ) ;
#2092 = FACE_OUTER_BOUND ( 'NONE', #1056, .T. ) ;
#2093 = ORIENTED_EDGE ( 'NONE', *, *, #2109, .T. ) ;
#2094 = CARTESIAN_POINT ( 'NONE',  ( 8.336125322366124024, 21.45114114349586387, 7.948328953041721157 ) ) ;
#2095 = CARTESIAN_POINT ( 'NONE',  ( -2.436617367782499599, 22.87153588547686667, 24.67833651202806067 ) ) ;
#2096 = CARTESIAN_POINT ( 'NONE',  ( 2.985931097914281462, 24.82479382442820537, 9.752995572818681680 ) ) ;
#2097 = EDGE_CURVE ( 'NONE', #3522, #3657, #2320, .T. ) ;
#2098 = CARTESIAN_POINT ( 'NONE',  ( -6.500000000000000000, 130.6770782520313219, 12.00000000000000000 ) ) ;
#2099 = ORIENTED_EDGE ( 'NONE', *, *, #2473, .T. ) ;
#2100 = ORIENTED_EDGE ( 'NONE', *, *, #1443, .T. ) ;
#2101 = ORIENTED_EDGE ( 'NONE', *, *, #6012, .T. ) ;
#2102 = LINE ( 'NONE', #4547, #4454 ) ;
#2103 = ADVANCED_FACE ( 'NONE', ( #2728 ), #4705, .T. ) ;
#2104 = DIRECTION ( 'NONE',  ( -0.000000000000000000, 0.000000000000000000, 1.000000000000000000 ) ) ;
#2105 = FACE_OUTER_BOUND ( 'NONE', #2171, .T. ) ;
#2106 = PLANE ( 'NONE',  #900 ) ;
#2107 = DIRECTION ( 'NONE',  ( -0.000000000000000000, -0.000000000000000000, -1.000000000000000000 ) ) ;
#2108 = ORIENTED_EDGE ( 'NONE', *, *, #6223, .F. ) ;
#2109 = EDGE_CURVE ( 'NONE', #3061, #1339, #3747, .T. ) ;
#2110 = CIRCLE ( 'NONE', #5721, 17.00000000000000000 ) ;
#2111 = ADVANCED_FACE ( 'NONE', ( #3412 ), #4376, .T. ) ;
#2112 = DIRECTION ( 'NONE',  ( 1.000000000000000000, 0.000000000000000000, 0.000000000000000000 ) ) ;
#2113 = CARTESIAN_POINT ( 'NONE',  ( -17.00000000000000000, 2.081899558550500280E-15, -49.99999999999999289 ) ) ;
#2114 = ORIENTED_EDGE ( 'NONE', *, *, #69, .F. ) ;
#2115 = LINE ( 'NONE', #3656, #4215 ) ;
#2116 = EDGE_LOOP ( 'NONE', ( #134, #3194, #4226, #6055 ) ) ;
#2117 = ADVANCED_FACE ( 'NONE', ( #4343 ), #2962, .T. ) ;
#2118 = DIRECTION ( 'NONE',  ( -0.000000000000000000, -0.000000000000000000, -1.000000000000000000 ) ) ;
#2119 = DIRECTION ( 'NONE',  ( -0.000000000000000000, -0.000000000000000000, 1.000000000000000000 ) ) ;
#2120 = CYLINDRICAL_SURFACE ( 'NONE', #3370, 25.00000000000000000 ) ;
#2121 = CARTESIAN_POINT ( 'NONE',  ( 0.000000000000000000, 0.000000000000000000, 39.00000000000001421 ) ) ;
#2122 = ORIENTED_EDGE ( 'NONE', *, *, #1493, .T. ) ;
#2123 = EDGE_CURVE ( 'NONE', #1293, #4159, #1812, .T. ) ;
#2124 = AXIS2_PLACEMENT_3D ( 'NONE', #641, #451, #1414 ) ;
#2125 = CYLINDRICAL_SURFACE ( 'NONE', #4409, 25.00000000000000000 ) ;
#2126 = CARTESIAN_POINT ( 'NONE',  ( 2.226229255992760780, 22.89589894665499870, 24.59902000234163211 ) ) ;
#2127 = CARTESIAN_POINT ( 'NONE',  ( -8.983986218495344289, 23.34169575125378771, 7.586426789398493575 ) ) ;
#2128 = DIRECTION ( 'NONE',  ( -0.000000000000000000, -0.000000000000000000, -1.000000000000000000 ) ) ;
#2129 = ORIENTED_EDGE ( 'NONE', *, *, #1246, .T. ) ;
#2130 = VERTEX_POINT ( 'NONE', #5905 ) ;
#2131 = CIRCLE ( 'NONE', #6050, 23.00000000000000000 ) ;
#2132 = CARTESIAN_POINT ( 'NONE',  ( 0.000000000000000000, 0.000000000000000000, 51.00000000000002842 ) ) ;
#2133 = LINE ( 'NONE', #217, #1702 ) ;
#2134 = CARTESIAN_POINT ( 'NONE',  ( 3.122849337825746672E-15, 17.00000000000000000, 281.0000000000000000 ) ) ;
#2135 = CIRCLE ( 'NONE', #5129, 19.00000000000000000 ) ;
#2136 = CARTESIAN_POINT ( 'NONE',  ( 0.000000000000000000, 0.000000000000000000, 47.00000000000000711 ) ) ;
#2137 = PLANE ( 'NONE',  #1838 ) ;
#2138 = EDGE_LOOP ( 'NONE', ( #2348, #5071, #3428, #469 ) ) ;
#2139 = ORIENTED_EDGE ( 'NONE', *, *, #607, .T. ) ;
#2140 = CIRCLE ( 'NONE', #4302, 14.00000000000001243 ) ;
#2141 = ADVANCED_FACE ( 'NONE', ( #4865 ), #455, .F. ) ;
#2142 = DIRECTION ( 'NONE',  ( -0.000000000000000000, 1.000000000000000000, -0.000000000000000000 ) ) ;
#2143 = VERTEX_POINT ( 'NONE', #973 ) ;
#2144 = VECTOR ( 'NONE', #1022, 1000.000000000000000 ) ;
#2145 = PRODUCT ( 'Part 32,3_Varsay\X2\0131\X0\lan', 'Part 32,3_Varsay\X2\0131\X0\lan', '', ( #5566 ) ) ;
#2146 = FACE_OUTER_BOUND ( 'NONE', #1203, .T. ) ;
#2147 = EDGE_LOOP ( 'NONE', ( #3419, #5932 ) ) ;
#2148 = AXIS2_PLACEMENT_3D ( 'NONE', #5978, #2976, #4998 ) ;
#2149 = CARTESIAN_POINT ( 'NONE',  ( -44.64065620456893413, -28.99954194078699032, -45.00000000000000000 ) ) ;
#2150 = DIRECTION ( 'NONE',  ( -1.836970198721029194E-16, -1.000000000000000000, 0.000000000000000000 ) ) ;
#2151 = DIRECTION ( 'NONE',  ( -0.000000000000000000, -0.000000000000000000, -1.000000000000000000 ) ) ;
#2152 = VECTOR ( 'NONE', #3483, 1000.000000000000000 ) ;
#2153 = CARTESIAN_POINT ( 'NONE',  ( 44.64065620456912598, 28.99954194078667413, -65.00000000000000000 ) ) ;
#2154 = ORIENTED_EDGE ( 'NONE', *, *, #700, .F. ) ;
#2155 = CARTESIAN_POINT ( 'NONE',  ( -16.23652742703190199, -37.28747423195189015, -65.00000000000000000 ) ) ;
#2156 = CARTESIAN_POINT ( 'NONE',  ( 17.00000000000000000, 2.081899558550500280E-15, -175.0000000000000284 ) ) ;
#2157 = CARTESIAN_POINT ( 'NONE',  ( 1.127325861074953917, 22.97343572093476638, 24.35677350376877470 ) ) ;
#2158 = AXIS2_PLACEMENT_3D ( 'NONE', #6021, #6114, #5571 ) ;
#2159 = CARTESIAN_POINT ( 'NONE',  ( -7.127827911436782848, 23.96564785266029673, 8.515057432034145890 ) ) ;
#2160 = AXIS2_PLACEMENT_3D ( 'NONE', #3450, #2490, #952 ) ;
#2161 = CIRCLE ( 'NONE', #3191, 90.00000000000321165 ) ;
#2162 = CARTESIAN_POINT ( 'NONE',  ( 6.002163747819661666, -22.20348677930560655, 36.27767814654681899 ) ) ;
#2163 = EDGE_LOOP ( 'NONE', ( #1780, #1901, #2945, #1706 ) ) ;
#2164 = ORIENTED_EDGE ( 'NONE', *, *, #3324, .T. ) ;
#2165 = ORIENTED_EDGE ( 'NONE', *, *, #974, .T. ) ;
#2166 = FACE_OUTER_BOUND ( 'NONE', #2361, .T. ) ;
#2167 = CARTESIAN_POINT ( 'NONE',  ( 13.14183123006966980, -39.58265509608656174, -110.0000000000000000 ) ) ;
#2168 = CYLINDRICAL_SURFACE ( 'NONE', #1435, 67.50000000000000000 ) ;
#2169 =( REPRESENTATION_RELATIONSHIP ('NONE','NONE', #632, #1490 ) REPRESENTATION_RELATIONSHIP_WITH_TRANSFORMATION ( #2988 )SHAPE_REPRESENTATION_RELATIONSHIP( ) );
#2170 = CARTESIAN_POINT ( 'NONE',  ( 44.43364355155687662, -29.42304313293534790, -30.00000000000000000 ) ) ;
#2171 = EDGE_LOOP ( 'NONE', ( #1130, #2064, #6240, #4396 ) ) ;
#2172 =( NAMED_UNIT ( * ) SI_UNIT ( $, .STERADIAN. ) SOLID_ANGLE_UNIT ( ) );
#2173 = CARTESIAN_POINT ( 'NONE',  ( -6.810998761473115337, -21.97232263399875762, 8.650160397932937784 ) ) ;
#2174 = ORIENTED_EDGE ( 'NONE', *, *, #4687, .T. ) ;
#2175 = CARTESIAN_POINT ( 'NONE',  ( 0.000000000000000000, 25.00000000000000000, 31.77501000028010125 ) ) ;
#2176 = ORIENTED_EDGE ( 'NONE', *, *, #315, .F. ) ;
#2177 = CARTESIAN_POINT ( 'NONE',  ( 0.000000000000000000, 0.000000000000000000, -180.0000000000000000 ) ) ;
#2178 = CARTESIAN_POINT ( 'NONE',  ( 0.000000000000000000, 0.000000000000000000, 0.000000000000000000 ) ) ;
#2179 = CARTESIAN_POINT ( 'NONE',  ( 7.500000000000000000, 9.184850993605147944E-16, 47.00000000000000000 ) ) ;
#2180 = ADVANCED_FACE ( 'NONE', ( #4445 ), #2415, .T. ) ;
#2181 = CARTESIAN_POINT ( 'NONE',  ( -17.00000000000000355, -25.00000000000000000, -130.0000000000000000 ) ) ;
#2182 = FACE_OUTER_BOUND ( 'NONE', #34, .T. ) ;
#2183 = EDGE_LOOP ( 'NONE', ( #3037, #511 ) ) ;
#2184 = DIRECTION ( 'NONE',  ( 1.000000000000000000, 0.000000000000000000, 0.000000000000000000 ) ) ;
#2185 = VECTOR ( 'NONE', #3254, 1000.000000000000000 ) ;
#2186 = CARTESIAN_POINT ( 'NONE',  ( 107.0000000000000142, 69.00000000000000000, 110.0000000000000000 ) ) ;
#2187 = CARTESIAN_POINT ( 'NONE',  ( -21.00000000000000355, 0.000000000000000000, 16.00000000000000000 ) ) ;
#2188 = EDGE_CURVE ( 'NONE', #3554, #4831, #3344, .T. ) ;
#2189 = DIRECTION ( 'NONE',  ( 0.000000000000000000, -1.000000000000000000, 0.000000000000000000 ) ) ;
#2190 = DIRECTION ( 'NONE',  ( 0.000000000000000000, -0.000000000000000000, -1.000000000000000000 ) ) ;
#2191 = ORIENTED_EDGE ( 'NONE', *, *, #1640, .F. ) ;
#2192 = VERTEX_POINT ( 'NONE', #5391 ) ;
#2193 = ADVANCED_FACE ( 'NONE', ( #4415 ), #881, .F. ) ;
#2194 = DIRECTION ( 'NONE',  ( -0.000000000000000000, -0.000000000000000000, 1.000000000000000000 ) ) ;
#2195 = PRODUCT_DEFINITION_SHAPE ( 'NONE', 'NONE',  #6377 ) ;
#2196 = CARTESIAN_POINT ( 'NONE',  ( 0.000000000000000000, 0.000000000000000000, -20.00000000000000000 ) ) ;
#2197 = EDGE_CURVE ( 'NONE', #4930, #643, #3345, .T. ) ;
#2198 = LINE ( 'NONE', #1657, #5865 ) ;
#2199 = DIRECTION ( 'NONE',  ( -0.000000000000000000, -0.000000000000000000, -1.000000000000000000 ) ) ;
#2200 = EDGE_LOOP ( 'NONE', ( #6112, #2449, #1564, #4036 ) ) ;
#2201 = FACE_BOUND ( 'NONE', #3099, .T. ) ;
#2202 = ORIENTED_EDGE ( 'NONE', *, *, #2385, .F. ) ;
#2203 = EDGE_CURVE ( 'NONE', #3504, #5509, #3863, .T. ) ;
#2204 =( LENGTH_UNIT ( ) NAMED_UNIT ( * ) SI_UNIT ( .MILLI., .METRE. ) );
#2205 = CARTESIAN_POINT ( 'NONE',  ( 12.81154844869972997, -19.11229287055882864, 4.578663348692236568 ) ) ;
#2206 = VERTEX_POINT ( 'NONE', #1902 ) ;
#2207 = LINE ( 'NONE', #2751, #9 ) ;
#2208 = EDGE_LOOP ( 'NONE', ( #1463, #4499, #5951, #250 ) ) ;
#2209 = VECTOR ( 'NONE', #2142, 1000.000000000000000 ) ;
#2210 = CARTESIAN_POINT ( 'NONE',  ( 0.2052511266213299934, 21.25619793154162807, -30.00000000000000000 ) ) ;
#2211 = AXIS2_PLACEMENT_3D ( 'NONE', #5841, #530, #2827 ) ;
#2212 = CARTESIAN_POINT ( 'NONE',  ( 73.99999999999987210, 76.99999716619419132, 276.0000000000000000 ) ) ;
#2213 = CYLINDRICAL_SURFACE ( 'NONE', #4315, 7.500000000000000000 ) ;
#2214 = ORIENTED_EDGE ( 'NONE', *, *, #1817, .T. ) ;
#2215 = CARTESIAN_POINT ( 'NONE',  ( 2.239119884489100709, 22.89489171314753335, 9.863953455948397675 ) ) ;
#2216 = EDGE_LOOP ( 'NONE', ( #922, #2510, #570, #4157 ) ) ;
#2217 = DIRECTION ( 'NONE',  ( 1.000000000000000000, 0.000000000000000000, -0.000000000000000000 ) ) ;
#2218 = CARTESIAN_POINT ( 'NONE',  ( -3.061616997868383043E-15, -25.00000000000000000, -130.0000000000000000 ) ) ;
#2219 = VECTOR ( 'NONE', #4875, 1000.000000000000000 ) ;
#2220 = CIRCLE ( 'NONE', #2528, 90.00000000000000000 ) ;
#2221 = CIRCLE ( 'NONE', #1190, 46.00000000000000000 ) ;
#2222 = CARTESIAN_POINT ( 'NONE',  ( 6.505027467542590536, -22.06241888168487009, 35.53465933272089927 ) ) ;
#2223 = EDGE_LOOP ( 'NONE', ( #4071, #840 ) ) ;
#2224 = ORIENTED_EDGE ( 'NONE', *, *, #3409, .T. ) ;
#2225 = CARTESIAN_POINT ( 'NONE',  ( -6.724622458085280918, 24.07890901287612806, 35.10508533856560831 ) ) ;
#2226 = AXIS2_PLACEMENT_3D ( 'NONE', #3438, #3406, #5523 ) ;
#2227 = PLANE ( 'NONE',  #5322 ) ;
#2228 = CARTESIAN_POINT ( 'NONE',  ( 44.43364355155687662, -29.42304313293534790, -180.0000000000000000 ) ) ;
#2229 = LINE ( 'NONE', #2618, #6069 ) ;
#2230 = VECTOR ( 'NONE', #3613, 1000.000000000000000 ) ;
#2231 = VERTEX_POINT ( 'NONE', #2351 ) ;
#2232 = DIRECTION ( 'NONE',  ( 1.000000000000000000, 0.000000000000000000, 0.000000000000000000 ) ) ;
#2233 = ORIENTED_EDGE ( 'NONE', *, *, #2390, .F. ) ;
#2234 = COLOUR_RGB ( '',0.7921568627450980005, 0.8196078431372548767, 0.9333333333333333481 ) ;
#2235 = CARTESIAN_POINT ( 'NONE',  ( 15.99408614349810698, -16.52843635781563592, 0.000000000000000000 ) ) ;
#2236 = CARTESIAN_POINT ( 'NONE',  ( 13.86188709689055543, -18.36473791091104246, 3.388952392393740354 ) ) ;
#2237 = CARTESIAN_POINT ( 'NONE',  ( -2.385244779468109755E-15, -1.040834085586084257E-14, -115.0000000000000000 ) ) ;
#2238 = VERTEX_POINT ( 'NONE', #5877 ) ;
#2239 = CIRCLE ( 'NONE', #5859, 25.00000000000000000 ) ;
#2240 = CARTESIAN_POINT ( 'NONE',  ( 64.99991398172927859, 32.11307465182860454, 1.734723475976807094E-15 ) ) ;
#2241 = UNCERTAINTY_MEASURE_WITH_UNIT (LENGTH_MEASURE( 1.000000000000000082E-05 ), #3940, 'distance_accuracy_value', 'NONE');
#2242 = DIRECTION ( 'NONE',  ( 0.000000000000000000, 0.000000000000000000, 1.000000000000000000 ) ) ;
#2243 = DIRECTION ( 'NONE',  ( -1.000000000000000000, 1.852483853906148040E-16, 0.000000000000000000 ) ) ;
#2244 = VECTOR ( 'NONE', #454, 1000.000000000000000 ) ;
#2245 = CARTESIAN_POINT ( 'NONE',  ( 0.000000000000000000, 0.000000000000000000, 55.00000000000000711 ) ) ;
#2246 = CARTESIAN_POINT ( 'NONE',  ( -7.114947004179562384, -23.96699118800356842, 34.19833922271499915 ) ) ;
#2247 = VERTEX_POINT ( 'NONE', #4313 ) ;
#2249 = VERTEX_POINT ( 'NONE', #1382 ) ;
#2248 = AXIS2_PLACEMENT_3D ( 'NONE', #1270, #1785, #3231 ) ;
#2250 = AXIS2_PLACEMENT_3D ( 'NONE', #243, #1683, #5176 ) ;
#2251 = PLANE ( 'NONE',  #1454 ) ;
#2252 = DIRECTION ( 'NONE',  ( -0.000000000000000000, -0.000000000000000000, -1.000000000000000000 ) ) ;
#2253 = APPLICATION_CONTEXT ( 'automotive_design' ) ;
#2254 = DIRECTION ( 'NONE',  ( 1.224646799147353207E-16, 1.000000000000000000, -0.000000000000000000 ) ) ;
#2255 = CARTESIAN_POINT ( 'NONE',  ( 1.790150932673403750, -22.93126094008908566, 24.48831024192238814 ) ) ;
#2256 = ORIENTED_EDGE ( 'NONE', *, *, #2544, .T. ) ;
#2257 = ADVANCED_FACE ( 'NONE', ( #1972 ), #4834, .T. ) ;
#2258 = ORIENTED_EDGE ( 'NONE', *, *, #3409, .F. ) ;
#2259 = VECTOR ( 'NONE', #2026, 1000.000000000000000 ) ;
#2260 = CARTESIAN_POINT ( 'NONE',  ( -3.769188925537567236, 24.71764851934220530, 38.27740560533011660 ) ) ;
#2261 = AXIS2_PLACEMENT_3D ( 'NONE', #3122, #235, #5165 ) ;
#2262 = DIRECTION ( 'NONE',  ( 1.000000000000000000, 0.000000000000000000, 0.000000000000000000 ) ) ;
#2263 = DIRECTION ( 'NONE',  ( 1.734723475976809855E-15, 1.000000000000000000, 0.000000000000000000 ) ) ;
#2264 = CARTESIAN_POINT ( 'NONE',  ( -44.64065620456596406, -28.99954194078535963, -240.0000000000000000 ) ) ;
#2265 = EDGE_CURVE ( 'NONE', #5889, #1574, #5612, .T. ) ;
#2266 = ORIENTED_EDGE ( 'NONE', *, *, #3209, .T. ) ;
#2267 = ADVANCED_FACE ( 'NONE', ( #1456, #3962 ), #7, .T. ) ;
#2268 = VERTEX_POINT ( 'NONE', #1876 ) ;
#2269 = VECTOR ( 'NONE', #381, 1000.000000000000000 ) ;
#2270 = ADVANCED_FACE ( 'NONE', ( #5936 ), #5361, .T. ) ;
#2271 = EDGE_CURVE ( 'NONE', #1019, #686, #2621, .T. ) ;
#2272 = EDGE_CURVE ( 'NONE', #4999, #643, #135, .T. ) ;
#2273 = CARTESIAN_POINT ( 'NONE',  ( -2.239119884489100709, -22.89489171314753335, 9.863953455948397675 ) ) ;
#2274 = EDGE_LOOP ( 'NONE', ( #5039, #5820, #4176, #878, #6063, #4442 ) ) ;
#2275 = CARTESIAN_POINT ( 'NONE',  ( 0.000000000000000000, 0.000000000000000000, 110.0000000000000000 ) ) ;
#2276 = EDGE_LOOP ( 'NONE', ( #2997, #2928 ) ) ;
#2277 = CYLINDRICAL_SURFACE ( 'NONE', #3146, 17.00000000000000000 ) ;
#2278 =( NAMED_UNIT ( * ) PLANE_ANGLE_UNIT ( ) SI_UNIT ( $, .RADIAN. ) );
#2279 = CARTESIAN_POINT ( 'NONE',  ( 13.41482486054668399, 26.39531364385071655, 5.999999999999990230 ) ) ;
#2280 = EDGE_CURVE ( 'NONE', #6227, #371, #1394, .T. ) ;
#2281 = FACE_OUTER_BOUND ( 'NONE', #1131, .T. ) ;
#2282 = CARTESIAN_POINT ( 'NONE',  ( -5.952041157299176710, -24.28165242506072019, 36.34480154750762892 ) ) ;
#2283 = EDGE_LOOP ( 'NONE', ( #6128, #4516, #5663 ) ) ;
#2284 = DIRECTION ( 'NONE',  ( 0.000000000000000000, 0.000000000000000000, 1.000000000000000000 ) ) ;
#2285 = ORIENTED_EDGE ( 'NONE', *, *, #463, .F. ) ;
#2286 = DIRECTION ( 'NONE',  ( 0.000000000000000000, 0.000000000000000000, -1.000000000000000000 ) ) ;
#2287 = DIRECTION ( 'NONE',  ( 1.000000000000000000, 0.000000000000000000, 0.000000000000000000 ) ) ;
#2288 = FACE_OUTER_BOUND ( 'NONE', #1082, .T. ) ;
#2289 = CIRCLE ( 'NONE', #1475, 17.00000000000000000 ) ;
#2290 = CARTESIAN_POINT ( 'NONE',  ( 6.096488593930911470, -24.24566755320544686, 36.15017996222949392 ) ) ;
#2291 = EDGE_LOOP ( 'NONE', ( #5282, #5055, #3185, #1207 ) ) ;
#2292 = ORIENTED_EDGE ( 'NONE', *, *, #1612, .F. ) ;
#2293 = CARTESIAN_POINT ( 'NONE',  ( -7.257770128441432433, 23.92352318576052284, 33.72861583961352494 ) ) ;
#2294 = EDGE_CURVE ( 'NONE', #3869, #12, #4988, .T. ) ;
#2295 = LINE ( 'NONE', #2394, #3145 ) ;
#2296 = DIRECTION ( 'NONE',  ( 0.000000000000000000, 0.000000000000000000, 1.000000000000000000 ) ) ;
#2297 = CYLINDRICAL_SURFACE ( 'NONE', #2048, 17.00000000000000000 ) ;
#2298 = B_SPLINE_CURVE_WITH_KNOTS ( 'NONE', 3,
 ( #4939, #4873, #462, #915, #3420, #2869, #5459, #2491, #3968, #1040, #435, #4352, #1910, #3870, #5849, #953, #2422, #4996, #1158, #2610, #627, #3609, #143, #4571, #174, #5581, #1674, #5099, #4509, #563, #4538, #3575, #2037, #5608, #4479, #207, #2517, #2095, #4048, #1186, #3123, #3993, #75, #6096 ),
 .UNSPECIFIED., .F., .F.,
 ( 4, 2, 2, 2, 2, 2, 2, 2, 2, 2, 2, 2, 2, 2, 2, 2, 2, 2, 2, 2, 2, 4 ),
 ( 0.000000000000000000, 0.001348713335717714561, 0.002023070003576572708, 0.002697426671435430422, 0.004046140007153132406, 0.004720496675011990988, 0.005394853342870850436, 0.006743566678588568467, 0.007417923346447437456, 0.008092280014306306446, 0.009440993350024065242, 0.01078970668574182230, 0.01213842002145957069, 0.01281277668931844402, 0.01348713335717731908, 0.01483584669289507441, 0.01618456002861283147, 0.01753327336433058506, 0.01888198670004834212, 0.01955634336790721892, 0.02023070003576609918, 0.02157941337148385624 ),
 .UNSPECIFIED. ) ;
#2299 = ORIENTED_EDGE ( 'NONE', *, *, #707, .T. ) ;
#2300 = ORIENTED_EDGE ( 'NONE', *, *, #4480, .T. ) ;
#2301 = VERTEX_POINT ( 'NONE', #3026 ) ;
#2302 = EDGE_CURVE ( 'NONE', #1416, #2192, #3967, .T. ) ;
#2303 = EDGE_CURVE ( 'NONE', #2192, #3708, #5451, .T. ) ;
#2304 = DIRECTION ( 'NONE',  ( -1.000000000000000000, 0.000000000000000000, 0.000000000000000000 ) ) ;
#2305 = DIRECTION ( 'NONE',  ( 0.000000000000000000, 0.000000000000000000, -1.000000000000000000 ) ) ;
#2306 = ORIENTED_EDGE ( 'NONE', *, *, #4687, .F. ) ;
#2307 = DIRECTION ( 'NONE',  ( 0.000000000000000000, 0.000000000000000000, 1.000000000000000000 ) ) ;
#2308 = ORIENTED_EDGE ( 'NONE', *, *, #3611, .T. ) ;
#2309 = ADVANCED_FACE ( 'NONE', ( #620 ), #1571, .T. ) ;
#2310 = EDGE_CURVE ( 'NONE', #3367, #981, #5204, .T. ) ;
#2311 = PRESENTATION_STYLE_ASSIGNMENT (( #1800 ) ) ;
#2312 = DIRECTION ( 'NONE',  ( 0.000000000000000000, 0.000000000000000000, -1.000000000000000000 ) ) ;
#2313 = SHAPE_REPRESENTATION ( 'Part 32,1_Varsay\X2\0131\X0\lan', ( #6349 ), #389 ) ;
#2314 = DIRECTION ( 'NONE',  ( -1.000000000000000000, 0.000000000000000000, 0.000000000000000000 ) ) ;
#2315 = ADVANCED_FACE ( 'NONE', ( #5479 ), #4108, .T. ) ;
#2316 = CARTESIAN_POINT ( 'NONE',  ( -7.307255365082233389, -23.90829471491151281, 30.06775954199971679 ) ) ;
#2317 = ORIENTED_EDGE ( 'NONE', *, *, #5618, .F. ) ;
#2318 = FILL_AREA_STYLE_COLOUR ( '', #3278 ) ;
#2319 = DIRECTION ( 'NONE',  ( -0.000000000000000000, -0.000000000000000000, -1.000000000000000000 ) ) ;
#2320 = LINE ( 'NONE', #1776, #3111 ) ;
#2321 = CIRCLE ( 'NONE', #5934, 17.00000000000000000 ) ;
#2322 = ADVANCED_FACE ( 'NONE', ( #584 ), #1636, .T. ) ;
#2323 = DIRECTION ( 'NONE',  ( -1.000000000000000000, 0.000000000000000000, 0.000000000000000000 ) ) ;
#2324 = CARTESIAN_POINT ( 'NONE',  ( 6.493108461366341899, -24.14236833790515036, 35.53659098058280108 ) ) ;
#2325 = ORIENTED_EDGE ( 'NONE', *, *, #2353, .T. ) ;
#2326 = EDGE_LOOP ( 'NONE', ( #3283, #239 ) ) ;
#2327 = CARTESIAN_POINT ( 'NONE',  ( -7.115105366545458665, 23.96693872413611004, 34.19760250332532081 ) ) ;
#2328 = AXIS2_PLACEMENT_3D ( 'NONE', #409, #4325, #1365 ) ;
#2329 = VECTOR ( 'NONE', #3830, 1000.000000000000000 ) ;
#2330 = DIRECTION ( 'NONE',  ( -0.000000000000000000, 1.000000000000000000, -0.000000000000000000 ) ) ;
#2331 = FACE_OUTER_BOUND ( 'NONE', #2698, .T. ) ;
#2332 = DIRECTION ( 'NONE',  ( -0.000000000000000000, -0.000000000000000000, -1.000000000000000000 ) ) ;
#2333 = VERTEX_POINT ( 'NONE', #1083 ) ;
#2334 = ORIENTED_EDGE ( 'NONE', *, *, #1647, .T. ) ;
#2335 = CIRCLE ( 'NONE', #4592, 89.87058297576892585 ) ;
#2336 = VERTEX_POINT ( 'NONE', #3115 ) ;
#2337 = DIRECTION ( 'NONE',  ( -1.000000000000000000, 0.000000000000000000, 0.000000000000000000 ) ) ;
#2338 = DIRECTION ( 'NONE',  ( -0.000000000000000000, -0.000000000000000000, -1.000000000000000000 ) ) ;
#2339 = VECTOR ( 'NONE', #5809, 1000.000000000000000 ) ;
#2340 = CARTESIAN_POINT ( 'NONE',  ( -12.41746183823000393, 30.39531364385071655, 9.999999999999991118 ) ) ;
#2341 = ORIENTED_EDGE ( 'NONE', *, *, #1126, .F. ) ;
#2342 = VECTOR ( 'NONE', #3865, 1000.000000000000000 ) ;
#2343 = DIRECTION ( 'NONE',  ( -1.000000000000000000, 0.000000000000000000, 0.000000000000000000 ) ) ;
#2344 = CARTESIAN_POINT ( 'NONE',  ( 0.000000000000000000, 0.000000000000000000, 39.00000000000001421 ) ) ;
#2345 = LINE ( 'NONE', #4698, #2837 ) ;
#2346 = VECTOR ( 'NONE', #1759, 1000.000000000000000 ) ;
#2347 = CARTESIAN_POINT ( 'NONE',  ( -1.957493960826122814, -24.92801652726308248, 39.03205219918674374 ) ) ;
#2348 = ORIENTED_EDGE ( 'NONE', *, *, #3619, .F. ) ;
#2349 = EDGE_CURVE ( 'NONE', #643, #4930, #5313, .T. ) ;
#2350 = CARTESIAN_POINT ( 'NONE',  ( 3.769534566620170057, 24.71760338780762822, 38.27724873576354980 ) ) ;
#2351 = CARTESIAN_POINT ( 'NONE',  ( 8.000000000000007105, 72.93807001241029297, 9.999999999999996447 ) ) ;
#2352 = CIRCLE ( 'NONE', #5962, 22.67164836619070911 ) ;
#2353 = EDGE_CURVE ( 'NONE', #3234, #4844, #2929, .T. ) ;
#2354 = EDGE_CURVE ( 'NONE', #5057, #1144, #4018, .T. ) ;
#2355 = LINE ( 'NONE', #4316, #2339 ) ;
#2356 = CIRCLE ( 'NONE', #2466, 40.00000002749906258 ) ;
#2357 = CARTESIAN_POINT ( 'NONE',  ( 7.499773188859401252, -23.84855136421925081, 31.27916535100970563 ) ) ;
#2358 = ORIENTED_EDGE ( 'NONE', *, *, #3393, .T. ) ;
#2359 = VECTOR ( 'NONE', #3620, 1000.000000000000000 ) ;
#2360 = CARTESIAN_POINT ( 'NONE',  ( 197.0000000000000000, 68.99999999999997158, 110.0000000000000000 ) ) ;
#2361 = EDGE_LOOP ( 'NONE', ( #6122, #5009, #4149, #3249 ) ) ;
#2362 = CARTESIAN_POINT ( 'NONE',  ( 265.0000000000000000, 14.00000000000000000, 110.0000000000000000 ) ) ;
#2363 = VECTOR ( 'NONE', #3514, 1000.000000000000000 ) ;
#2364 = LINE ( 'NONE', #1392, #690 ) ;
#2365 = CARTESIAN_POINT ( 'NONE',  ( -12.41746183823000393, 30.39531364385071299, 1.999999999999990008 ) ) ;
#2366 = DIRECTION ( 'NONE',  ( 0.000000000000000000, -1.000000000000000000, 0.000000000000000000 ) ) ;
#2367 = AXIS2_PLACEMENT_3D ( 'NONE', #839, #3794, #2818 ) ;
#2368 = VERTEX_POINT ( 'NONE', #3540 ) ;
#2369 = EDGE_LOOP ( 'NONE', ( #1828, #45, #1716, #2292 ) ) ;
#2370 = DIRECTION ( 'NONE',  ( -0.000000000000000000, -0.000000000000000000, -1.000000000000000000 ) ) ;
#2371 = CIRCLE ( 'NONE', #4845, 22.67164836619070911 ) ;
#2372 = DIRECTION ( 'NONE',  ( -1.000000000000000000, 0.000000000000000000, 0.000000000000000000 ) ) ;
#2373 = AXIS2_PLACEMENT_3D ( 'NONE', #2402, #6308, #2910 ) ;
#2374 = DIRECTION ( 'NONE',  ( 1.000000000000000000, 0.000000000000000000, -0.000000000000000000 ) ) ;
#2375 = ORIENTED_EDGE ( 'NONE', *, *, #191, .T. ) ;
#2376 = CARTESIAN_POINT ( 'NONE',  ( -5.722301980643075048, -22.27724803853372393, 26.92170784547232998 ) ) ;
#2377 = EDGE_CURVE ( 'NONE', #3651, #3949, #2523, .T. ) ;
#2378 = DIRECTION ( 'NONE',  ( -0.000000000000000000, 0.000000000000000000, -1.000000000000000000 ) ) ;
#2379 = APPLICATION_CONTEXT ( 'automotive_design' ) ;
#2380 = CARTESIAN_POINT ( 'NONE',  ( -4.956647734651107307, -24.50626513604597889, 37.42488445140200071 ) ) ;
#2381 = EDGE_LOOP ( 'NONE', ( #2736, #407, #4709, #3732 ) ) ;
#2382 = DIRECTION ( 'NONE',  ( -1.000000000000000000, 0.000000000000000000, 0.000000000000000000 ) ) ;
#2383 = CIRCLE ( 'NONE', #5380, 22.67164836619068424 ) ;
#2384 = DIRECTION ( 'NONE',  ( 1.000000000000000000, 0.000000000000000000, 0.000000000000000000 ) ) ;
#2385 = EDGE_CURVE ( 'NONE', #3758, #5846, #6129, .T. ) ;
#2386 = DIRECTION ( 'NONE',  ( 0.000000000000000000, 0.000000000000000000, -1.000000000000000000 ) ) ;
#2387 = CARTESIAN_POINT ( 'NONE',  ( 1.948881123199609489, -24.92505092879369499, 24.52843033598425393 ) ) ;
#2388 = VERTEX_POINT ( 'NONE', #2030 ) ;
#2389 = CARTESIAN_POINT ( 'NONE',  ( 44.00000000000000000, -13.41640786499874771, 15.00000000000000000 ) ) ;
#2390 = EDGE_CURVE ( 'NONE', #1273, #1953, #2110, .T. ) ;
#2391 = ORIENTED_EDGE ( 'NONE', *, *, #405, .T. ) ;
#2392 = PLANE ( 'NONE',  #5588 ) ;
#2393 = EDGE_CURVE ( 'NONE', #624, #6099, #992, .T. ) ;
#2394 = CARTESIAN_POINT ( 'NONE',  ( -17.00000000000000000, 2.081899558550500280E-15, -273.0000000000000000 ) ) ;
#2395 = AXIS2_PLACEMENT_3D ( 'NONE', #1492, #1884, #5397 ) ;
#2396 = CARTESIAN_POINT ( 'NONE',  ( -25.00000000000000000, 0.000000000000000000, 41.00000000000000000 ) ) ;
#2397 = CARTESIAN_POINT ( 'NONE',  ( 8.000000000000003553, 100.3953136438507272, 1.999999999999998224 ) ) ;
#2398 = EDGE_CURVE ( 'NONE', #5912, #4340, #3774, .T. ) ;
#2399 = ORIENTED_EDGE ( 'NONE', *, *, #4211, .F. ) ;
#2400 = ORIENTED_EDGE ( 'NONE', *, *, #1406, .T. ) ;
#2401 = EDGE_CURVE ( 'NONE', #6280, #4815, #5212, .T. ) ;
#2402 = CARTESIAN_POINT ( 'NONE',  ( 0.000000000000000000, 0.000000000000000000, 16.00000000000000000 ) ) ;
#2403 = CARTESIAN_POINT ( 'NONE',  ( 0.000000000000000000, 25.00000000000000000, -7.790539539321167162 ) ) ;
#2404 = ADVANCED_FACE ( 'NONE', ( #1769 ), #2277, .T. ) ;
#2405 = CARTESIAN_POINT ( 'NONE',  ( 17.05141243254541550, -24.25762350764758679, 12.00000000000000000 ) ) ;
#2406 = ORIENTED_EDGE ( 'NONE', *, *, #2776, .F. ) ;
#2407 = ORIENTED_EDGE ( 'NONE', *, *, #3338, .T. ) ;
#2408 = DIRECTION ( 'NONE',  ( -0.000000000000000000, -0.000000000000000000, -1.000000000000000000 ) ) ;
#2409 = DIRECTION ( 'NONE',  ( 2.668808879446237100E-17, -1.000000000000000000, -3.081487911019577365E-33 ) ) ;
#2410 = CARTESIAN_POINT ( 'NONE',  ( -5.266685217916866613, -22.38944685319058436, 26.43066030061579141 ) ) ;
#2411 = DIRECTION ( 'NONE',  ( 1.000000000000000000, 0.000000000000000000, 0.000000000000000000 ) ) ;
#2412 = LINE ( 'NONE', #2477, #1125 ) ;
#2413 = ORIENTED_EDGE ( 'NONE', *, *, #4360, .T. ) ;
#2414 = CARTESIAN_POINT ( 'NONE',  ( 9.184177739184520255E-16, -25.00000000000000000, 39.27501000028010480 ) ) ;
#2415 = CYLINDRICAL_SURFACE ( 'NONE', #60, 17.00000000000000000 ) ;
#2416 = DIRECTION ( 'NONE',  ( -1.000000000000000000, -0.000000000000000000, -0.000000000000000000 ) ) ;
#2417 = DIRECTION ( 'NONE',  ( -0.000000000000000000, -0.000000000000000000, -1.000000000000000000 ) ) ;
#2418 = ORIENTED_EDGE ( 'NONE', *, *, #2673, .F. ) ;
#2419 = DIRECTION ( 'NONE',  ( -1.836970198721029194E-16, -1.000000000000000000, 0.000000000000000000 ) ) ;
#2420 = CARTESIAN_POINT ( 'NONE',  ( 13.05961095629095503, 27.77190499716703798, 9.030829679283289835 ) ) ;
#2421 = AXIS2_PLACEMENT_3D ( 'NONE', #4471, #3568, #4597 ) ;
#2422 = CARTESIAN_POINT ( 'NONE',  ( -7.059519746509402616, 21.88992045406459042, 34.31748813447425306 ) ) ;
#2423 = CIRCLE ( 'NONE', #5415, 22.67164836619067714 ) ;
#2424 = CYLINDRICAL_SURFACE ( 'NONE', #2328, 25.00000000000000000 ) ;
#2425 = CARTESIAN_POINT ( 'NONE',  ( 0.000000000000000000, 0.000000000000000000, 281.0000000000000000 ) ) ;
#2426 = DIRECTION ( 'NONE',  ( -0.000000000000000000, -0.000000000000000000, -1.000000000000000000 ) ) ;
#2427 = ORIENTED_EDGE ( 'NONE', *, *, #968, .T. ) ;
#2428 = ORIENTED_EDGE ( 'NONE', *, *, #2385, .T. ) ;
#2429 = ORIENTED_EDGE ( 'NONE', *, *, #5467, .T. ) ;
#2430=STYLED_ITEM('',(#6419),#2488);
#2431 = DIRECTION ( 'NONE',  ( -0.000000000000000000, -0.000000000000000000, -1.000000000000000000 ) ) ;
#2432 = CIRCLE ( 'NONE', #5418, 12.50000000000001421 ) ;
#2433 = DIRECTION ( 'NONE',  ( -0.000000000000000000, -0.000000000000000000, -1.000000000000000000 ) ) ;
#2434 = FACE_OUTER_BOUND ( 'NONE', #2515, .T. ) ;
#2435 = EDGE_LOOP ( 'NONE', ( #2497, #3811, #4869, #3341 ) ) ;
#2436 = AXIS2_PLACEMENT_3D ( 'NONE', #5013, #5498, #551 ) ;
#2437 =( LENGTH_UNIT ( ) NAMED_UNIT ( * ) SI_UNIT ( .MILLI., .METRE. ) );
#2438 = CARTESIAN_POINT ( 'NONE',  ( 0.000000000000000000, 0.000000000000000000, 15.00000000000000000 ) ) ;
#2439 = FACE_OUTER_BOUND ( 'NONE', #534, .T. ) ;
#2440 = DIRECTION ( 'NONE',  ( -0.000000000000000000, -0.000000000000000000, -1.000000000000000000 ) ) ;
#2441 = ORIENTED_EDGE ( 'NONE', *, *, #2302, .F. ) ;
#2442 = CARTESIAN_POINT ( 'NONE',  ( 2.380270672502711906E-15, -5.204170427930421283E-15, -180.0000000000000000 ) ) ;
#2443 = VECTOR ( 'NONE', #1703, 1000.000000000000000 ) ;
#2444 = DIRECTION ( 'NONE',  ( -1.000000000000000000, 0.000000000000000000, 0.000000000000000000 ) ) ;
#2445 = CARTESIAN_POINT ( 'NONE',  ( 5.649026277996902046, 24.35594688685564790, 26.81770774654597034 ) ) ;
#2446 = AXIS2_PLACEMENT_3D ( 'NONE', #2019, #1924, #1476 ) ;
#2447 = CARTESIAN_POINT ( 'NONE',  ( -13.38023260448825447, 26.52727575619375244, 4.947004611186087253 ) ) ;
#2448 = CARTESIAN_POINT ( 'NONE',  ( 0.2456693407522394235, -24.99999999999999645, 39.27501000028009770 ) ) ;
#2449 = ORIENTED_EDGE ( 'NONE', *, *, #2082, .F. ) ;
#2450 = CARTESIAN_POINT ( 'NONE',  ( 4.378668635177231927, 22.59503479412315485, 9.474032806803469597 ) ) ;
#2451 = AXIS2_PLACEMENT_3D ( 'NONE', #3448, #4421, #2969 ) ;
#2452 = VERTEX_POINT ( 'NONE', #4630 ) ;
#2453 = DIRECTION ( 'NONE',  ( -1.000000000000000000, 0.000000000000000000, 0.000000000000000000 ) ) ;
#2454 = DIRECTION ( 'NONE',  ( 0.000000000000000000, 0.000000000000000000, -1.000000000000000000 ) ) ;
#2455 = LINE ( 'NONE', #1578, #5012 ) ;
#2456 = CIRCLE ( 'NONE', #2975, 17.00000000000000000 ) ;
#2457 = DIRECTION ( 'NONE',  ( 0.000000000000000000, 1.740526192617802767E-17, -1.000000000000000000 ) ) ;
#2458 = EDGE_LOOP ( 'NONE', ( #5298, #6141, #3579, #5465 ) ) ;
#2459 = ORIENTED_EDGE ( 'NONE', *, *, #579, .T. ) ;
#2460 = ORIENTED_EDGE ( 'NONE', *, *, #1596, .T. ) ;
#2461 = VERTEX_POINT ( 'NONE', #2240 ) ;
#2462 = VECTOR ( 'NONE', #2199, 1000.000000000000000 ) ;
#2463 = DIRECTION ( 'NONE',  ( -1.000000000000000000, 0.000000000000000000, 0.000000000000000000 ) ) ;
#2464 = EDGE_CURVE ( 'NONE', #5105, #4627, #5637, .T. ) ;
#2465 = CARTESIAN_POINT ( 'NONE',  ( 0.000000000000000000, 134.5953136438507158, 12.00000000000000000 ) ) ;
#2466 = AXIS2_PLACEMENT_3D ( 'NONE', #5487, #2550, #113 ) ;
#2467 = ADVANCED_FACE ( 'NONE', ( #5600 ), #3701, .F. ) ;
#2468 = CARTESIAN_POINT ( 'NONE',  ( 14.34088693563092853, -20.48519421429849174, 2.767956487184815462 ) ) ;
#2469 = EDGE_CURVE ( 'NONE', #5596, #3088, #2944, .T. ) ;
#2470 = ORIENTED_EDGE ( 'NONE', *, *, #264, .F. ) ;
#2471 = AXIS2_PLACEMENT_3D ( 'NONE', #4207, #2307, #252 ) ;
#2472 = EDGE_CURVE ( 'NONE', #2613, #1537, #4799, .T. ) ;
#2473 = EDGE_CURVE ( 'NONE', #1030, #590, #3737, .T. ) ;
#2474 = CARTESIAN_POINT ( 'NONE',  ( 66.31180517104782268, 102.2453362568401474, 162.8064542903391327 ) ) ;
#2475 = LINE ( 'NONE', #3473, #2587 ) ;
#2476 = CIRCLE ( 'NONE', #5781, 166.8359700257217071 ) ;
#2477 = CARTESIAN_POINT ( 'NONE',  ( 197.0000000000000000, 68.99999999999997158, 0.000000000000000000 ) ) ;
#2478 = ORIENTED_EDGE ( 'NONE', *, *, #187, .T. ) ;
#2479 = DIRECTION ( 'NONE',  ( 1.000000000000000000, 0.000000000000000000, 0.000000000000000000 ) ) ;
#2480 = CIRCLE ( 'NONE', #2883, 14.00000000000000000 ) ;
#2481 = DIRECTION ( 'NONE',  ( -0.000000000000000000, -0.000000000000000000, -1.000000000000000000 ) ) ;
#2482 = CARTESIAN_POINT ( 'NONE',  ( 4.574685241957344495, 24.57863749249463936, 25.82670804586578228 ) ) ;
#2483 = EDGE_CURVE ( 'NONE', #602, #3628, #2835, .T. ) ;
#2484 = PLANE ( 'NONE',  #2038 ) ;
#2485 = AXIS2_PLACEMENT_3D ( 'NONE', #1836, #359, #2821 ) ;
#2486 = CARTESIAN_POINT ( 'NONE',  ( -44.64065620456596406, -28.99954194078535963, -240.0000000000000000 ) ) ;
#2487 = VERTEX_POINT ( 'NONE', #4731 ) ;
#2488 = MANIFOLD_SOLID_BREP ( 'Fillet1', #1551 ) ;
#2489 = CARTESIAN_POINT ( 'NONE',  ( 19.25293315802893801, 8.385974291188240670, 12.00000000000000000 ) ) ;
#2490 = DIRECTION ( 'NONE',  ( -0.000000000000000000, -0.000000000000000000, -1.000000000000000000 ) ) ;
#2491 = CARTESIAN_POINT ( 'NONE',  ( -4.782950468712823699, 22.50022147858462418, 37.56939778472803226 ) ) ;
#2492 = FACE_BOUND ( 'NONE', #1284, .T. ) ;
#2493 = DIRECTION ( 'NONE',  ( 1.000000000000000000, 0.000000000000000000, 0.000000000000000000 ) ) ;
#2494 = CARTESIAN_POINT ( 'NONE',  ( 7.947562104483774093, 68.75545066608756883, 9.999999999999996447 ) ) ;
#2495 = ORIENTED_EDGE ( 'NONE', *, *, #4184, .F. ) ;
#2496 = ORIENTED_EDGE ( 'NONE', *, *, #4314, .F. ) ;
#2497 = ORIENTED_EDGE ( 'NONE', *, *, #4758, .F. ) ;
#2498 = VERTEX_POINT ( 'NONE', #1179 ) ;
#2499 = EDGE_CURVE ( 'NONE', #2535, #5649, #3250, .T. ) ;
#2500 = CARTESIAN_POINT ( 'NONE',  ( 0.000000000000000000, 120.0000000000000000, 12.00000000000000000 ) ) ;
#2501 = DIRECTION ( 'NONE',  ( 1.000000000000000000, -1.836970198721029194E-16, 0.000000000000000000 ) ) ;
#2502 = AXIS2_PLACEMENT_3D ( 'NONE', #1259, #236, #3805 ) ;
#2503 = CARTESIAN_POINT ( 'NONE',  ( -8.206466222643920005, -23.61787042823059224, 7.999630148859495193 ) ) ;
#2504 = EDGE_LOOP ( 'NONE', ( #3300, #404, #832, #5496 ) ) ;
#2505 = ADVANCED_FACE ( 'NONE', ( #2915 ), #3888, .T. ) ;
#2506 = DIRECTION ( 'NONE',  ( -0.000000000000000000, -0.000000000000000000, 1.000000000000000000 ) ) ;
#2507 = FACE_OUTER_BOUND ( 'NONE', #441, .T. ) ;
#2508 = EDGE_CURVE ( 'NONE', #4629, #4930, #3797, .T. ) ;
#2509 = CYLINDRICAL_SURFACE ( 'NONE', #628, 90.00000000000000000 ) ;
#2510 = ORIENTED_EDGE ( 'NONE', *, *, #1452, .F. ) ;
#2511 = DIRECTION ( 'NONE',  ( -1.000000000000000000, 0.000000000000000000, 0.000000000000000000 ) ) ;
#2512 = DIRECTION ( 'NONE',  ( -0.000000000000000000, -0.000000000000000000, 1.000000000000000000 ) ) ;
#2513 = CARTESIAN_POINT ( 'NONE',  ( 0.000000000000000000, 17.00000000000000000, 5.000000000000004441 ) ) ;
#2514 = CARTESIAN_POINT ( 'NONE',  ( 82.00000000000001421, 69.00000000000000000, 0.000000000000000000 ) ) ;
#2515 = EDGE_LOOP ( 'NONE', ( #4366, #4186 ) ) ;
#2516 = LINE ( 'NONE', #5848, #2879 ) ;
#2517 = CARTESIAN_POINT ( 'NONE',  ( -3.063555513103408678, 22.79893987554409662, 24.91467890029023025 ) ) ;
#2518 = DIRECTION ( 'NONE',  ( -0.000000000000000000, -0.000000000000000000, -1.000000000000000000 ) ) ;
#2519 = CARTESIAN_POINT ( 'NONE',  ( 16.99999999999999645, -24.99999999999999645, -130.0000000000000000 ) ) ;
#2520 = ORIENTED_EDGE ( 'NONE', *, *, #4682, .T. ) ;
#2521 = EDGE_LOOP ( 'NONE', ( #4233, #4816, #3843, #1677, #800, #6297, #3877, #2191, #3860 ) ) ;
#2522 = CARTESIAN_POINT ( 'NONE',  ( 16.23652742703164975, 37.28747423195200383, -45.00000000000000000 ) ) ;
#2523 = CIRCLE ( 'NONE', #1289, 25.00000000000000000 ) ;
#2524 = LINE ( 'NONE', #3042, #1538 ) ;
#2525 = DIRECTION ( 'NONE',  ( -1.000000000000000000, -1.852483853906148286E-16, 0.000000000000000000 ) ) ;
#2526 = ORIENTED_EDGE ( 'NONE', *, *, #1799, .T. ) ;
#2527 = CIRCLE ( 'NONE', #3561, 166.8359700257217071 ) ;
#2528 = AXIS2_PLACEMENT_3D ( 'NONE', #998, #5897, #4406 ) ;
#2529 = DIRECTION ( 'NONE',  ( 3.976288500601801518E-16, 3.618850321705485689E-16, 1.000000000000000000 ) ) ;
#2530 = FACE_OUTER_BOUND ( 'NONE', #1276, .T. ) ;
#2531 = VECTOR ( 'NONE', #392, 1000.000000000000000 ) ;
#2532 = EDGE_CURVE ( 'NONE', #3626, #3948, #5729, .T. ) ;
#2533 = CARTESIAN_POINT ( 'NONE',  ( 0.000000000000000000, 0.000000000000000000, 44.00000000000000711 ) ) ;
#2534 = ORIENTED_EDGE ( 'NONE', *, *, #3343, .T. ) ;
#2535 = VERTEX_POINT ( 'NONE', #873 ) ;
#2536 = AXIS2_PLACEMENT_3D ( 'NONE', #1837, #3799, #2559 ) ;
#2537 = DIRECTION ( 'NONE',  ( -1.000000000000000000, 0.000000000000000000, 0.000000000000000000 ) ) ;
#2538 = DIRECTION ( 'NONE',  ( -1.000000000000000000, 0.000000000000000000, 0.000000000000000000 ) ) ;
#2539 = VECTOR ( 'NONE', #78, 1000.000000000000000 ) ;
#2540 = EDGE_CURVE ( 'NONE', #5896, #2231, #4336, .T. ) ;
#2541 = CARTESIAN_POINT ( 'NONE',  ( 2.380270672502711906E-15, -5.204170427930421283E-15, -45.00000000000000000 ) ) ;
#2542 = EDGE_LOOP ( 'NONE', ( #2907, #253, #4729, #2586 ) ) ;
#2543 = CARTESIAN_POINT ( 'NONE',  ( 13.09536939405042055, 18.91069771112636744, 4.258167217702273355 ) ) ;
#2544 = EDGE_CURVE ( 'NONE', #4961, #3357, #5323, .T. ) ;
#2545 = DIRECTION ( 'NONE',  ( 1.000000000000000000, 0.000000000000000000, 0.000000000000000000 ) ) ;
#2546 = CARTESIAN_POINT ( 'NONE',  ( 7.267038029898874818, 21.82227126734110456, 29.86717584346564180 ) ) ;
#2547 = EDGE_CURVE ( 'NONE', #1278, #3016, #1820, .T. ) ;
#2548 = EDGE_CURVE ( 'NONE', #4328, #1077, #2220, .T. ) ;
#2549 = DIRECTION ( 'NONE',  ( 1.000000000000000000, -1.836970198721029194E-16, 0.000000000000000000 ) ) ;
#2550 = DIRECTION ( 'NONE',  ( 0.000000000000000000, -1.000000000000000000, 0.000000000000000000 ) ) ;
#2551 = VECTOR ( 'NONE', #6320, 1000.000000000000000 ) ;
#2552 = ORIENTED_EDGE ( 'NONE', *, *, #4011, .T. ) ;
#2553 = ORIENTED_EDGE ( 'NONE', *, *, #1156, .T. ) ;
#2554 = ORIENTED_EDGE ( 'NONE', *, *, #6304, .T. ) ;
#2555 = DIRECTION ( 'NONE',  ( -0.000000000000000000, -0.000000000000000000, -1.000000000000000000 ) ) ;
#2556 = CIRCLE ( 'NONE', #3375, 90.00000000000321165 ) ;
#2557 = DIRECTION ( 'NONE',  ( -0.000000000000000000, -0.000000000000000000, -1.000000000000000000 ) ) ;
#2558 = CARTESIAN_POINT ( 'NONE',  ( 0.000000000000000000, 0.000000000000000000, 1.000000000000000888 ) ) ;
#2559 = DIRECTION ( 'NONE',  ( -1.000000000000000000, 0.000000000000000000, 0.000000000000000000 ) ) ;
#2560 = DIRECTION ( 'NONE',  ( -0.000000000000000000, -0.000000000000000000, -1.000000000000000000 ) ) ;
#2561 = ORIENTED_EDGE ( 'NONE', *, *, #5104, .F. ) ;
#2562 = AXIS2_PLACEMENT_3D ( 'NONE', #4953, #2501, #4461 ) ;
#2563 = AXIS2_PLACEMENT_3D ( 'NONE', #4050, #5610, #788 ) ;
#2564 = CARTESIAN_POINT ( 'NONE',  ( -122.6881948289522342, 82.87638965790928580, 249.4579780890706218 ) ) ;
#2565 = CARTESIAN_POINT ( 'NONE',  ( 174.7835321302054865, 68.75545066608756883, 9.999999999999996447 ) ) ;
#2566 = DIRECTION ( 'NONE',  ( -0.000000000000000000, -0.000000000000000000, 1.000000000000000000 ) ) ;
#2567 = ORIENTED_EDGE ( 'NONE', *, *, #4871, .F. ) ;
#2568 = AXIS2_PLACEMENT_3D ( 'NONE', #4441, #2440, #5963 ) ;
#2569 = DIRECTION ( 'NONE',  ( 0.000000000000000000, 0.000000000000000000, -1.000000000000000000 ) ) ;
#2570 = EDGE_CURVE ( 'NONE', #1537, #2613, #5420, .T. ) ;
#2571 = DIRECTION ( 'NONE',  ( -0.000000000000000000, -0.000000000000000000, -1.000000000000000000 ) ) ;
#2572 = DIRECTION ( 'NONE',  ( -0.000000000000000000, -0.000000000000000000, 1.000000000000000000 ) ) ;
#2573 = EDGE_LOOP ( 'NONE', ( #2154, #148, #509, #3829 ) ) ;
#2574 = MECHANICAL_DESIGN_GEOMETRIC_PRESENTATION_REPRESENTATION (  '', ( #1761 ), #5268 ) ;
#2575 = VECTOR ( 'NONE', #833, 1000.000000000000000 ) ;
#2576 = CARTESIAN_POINT ( 'NONE',  ( 12.25547752887834818, 19.46581264560981239, 5.111654144181065895 ) ) ;
#2577 = EDGE_CURVE ( 'NONE', #2747, #1569, #3463, .T. ) ;
#2578 = FACE_BOUND ( 'NONE', #5796, .T. ) ;
#2579 = CARTESIAN_POINT ( 'NONE',  ( 7.412736743525290883, 21.77298136741688950, 33.00284858769864371 ) ) ;
#2580 = CARTESIAN_POINT ( 'NONE',  ( -11.91160812950987946, 21.98255961136171877, 5.429893957167271523 ) ) ;
#2581 = FACE_OUTER_BOUND ( 'NONE', #4107, .T. ) ;
#2582 = EDGE_CURVE ( 'NONE', #959, #4936, #1869, .T. ) ;
#2583 = ORIENTED_EDGE ( 'NONE', *, *, #529, .F. ) ;
#2584 = ORIENTED_EDGE ( 'NONE', *, *, #230, .T. ) ;
#2585 = ADVANCED_FACE ( 'NONE', ( #3433 ), #4367, .T. ) ;
#2586 = ORIENTED_EDGE ( 'NONE', *, *, #2203, .F. ) ;
#2587 = VECTOR ( 'NONE', #1993, 1000.000000000000000 ) ;
#2588 = DIRECTION ( 'NONE',  ( 1.000000000000000000, 0.000000000000000000, 0.000000000000000000 ) ) ;
#2589 = CYLINDRICAL_SURFACE ( 'NONE', #6186, 17.00000000000000000 ) ;
#2590 = CARTESIAN_POINT ( 'NONE',  ( 0.000000000000000000, 0.000000000000000000, 23.00000000000000000 ) ) ;
#2591 = EDGE_CURVE ( 'NONE', #713, #4635, #6338, .T. ) ;
#2592 = DIRECTION ( 'NONE',  ( 2.295390878742131754E-32, -1.239088197126290570E-16, 1.000000000000000000 ) ) ;
#2593 = B_SPLINE_CURVE_WITH_KNOTS ( 'NONE', 3,
 ( #6126, #4084, #5582, #629, #4672, #210, #4572, #1092, #2580, #2640, #3640, #2127, #2674, #2159, #3124, #176, #4118, #6097, #5100, #4539, #2701, #5609, #6070, #758, #144, #2096, #3577, #2611, #3673, #3097, #4049, #1614, #5034, #3067, #692, #1189, #265, #3158, #5647, #6158, #5550, #5130, #4182, #4642, #5067, #1226 ),
 .UNSPECIFIED., .F., .F.,
 ( 4, 2, 2, 2, 2, 2, 2, 2, 2, 2, 2, 2, 2, 2, 2, 2, 2, 2, 2, 2, 2, 2, 4 ),
 ( 4.230440722825154659E-18, 0.002589099528182561144, 0.005178199056365117951, 0.006472748820456394186, 0.007767298584547670422, 0.01035639811273022376, 0.01294549764091277796, 0.01424004740500405854, 0.01553459716909533911, 0.01812369669727790025, 0.01941824646136917909, 0.02071279622546045793, 0.02330189575364301907, 0.02459644551773429791, 0.02589099528182557675, 0.02848009481000812748, 0.02977464457409940632, 0.03106919433819068516, 0.03365829386637324283, 0.03495284363046452514, 0.03624739339455580051, 0.03883649292273835818, 0.04142559245092091585 ),
 .UNSPECIFIED. ) ;
#2594 = FACE_OUTER_BOUND ( 'NONE', #5822, .T. ) ;
#2595 = VERTEX_POINT ( 'NONE', #5801 ) ;
#2596 = CONTEXT_DEPENDENT_SHAPE_REPRESENTATION ( #3242, #2195 ) ;
#2597 = ADVANCED_FACE ( 'NONE', ( #1376 ), #3335, .T. ) ;
#2598 = SHAPE_DEFINITION_REPRESENTATION ( #2659, #3711 ) ;
#2599 = CARTESIAN_POINT ( 'NONE',  ( 25.00000000000000000, 3.061616997868383043E-15, 41.00000000000000000 ) ) ;
#2600 = ORIENTED_EDGE ( 'NONE', *, *, #1457, .F. ) ;
#2601 = DIRECTION ( 'NONE',  ( -0.000000000000000000, -0.000000000000000000, 1.000000000000000000 ) ) ;
#2602 = ORIENTED_EDGE ( 'NONE', *, *, #1911, .T. ) ;
#2603 = CARTESIAN_POINT ( 'NONE',  ( -44.64065620456893413, -28.99954194078699032, -45.00000000000000000 ) ) ;
#2604 = PLANE ( 'NONE',  #5275 ) ;
#2605 = DIRECTION ( 'NONE',  ( -0.000000000000000000, -0.000000000000000000, -1.000000000000000000 ) ) ;
#2606 = FACE_OUTER_BOUND ( 'NONE', #2643, .T. ) ;
#2607 = ORIENTED_EDGE ( 'NONE', *, *, #2401, .T. ) ;
#2608 = CARTESIAN_POINT ( 'NONE',  ( -4.711348314259845793, 22.51623045471248119, 9.370182291681606657 ) ) ;
#2609 = SURFACE_STYLE_FILL_AREA ( #2637 ) ;
#2610 = CARTESIAN_POINT ( 'NONE',  ( -7.411490251847205002, 21.77340291014862217, 33.00915547857365340 ) ) ;
#2611 = CARTESIAN_POINT ( 'NONE',  ( 4.258741324358275904, 24.63828325354172222, 9.488137494773077663 ) ) ;
#2612 = CARTESIAN_POINT ( 'NONE',  ( 0.000000000000000000, 0.000000000000000000, 0.000000000000000000 ) ) ;
#2613 = VERTEX_POINT ( 'NONE', #423 ) ;
#2614 = ORIENTED_EDGE ( 'NONE', *, *, #5232, .F. ) ;
#2615 = DIRECTION ( 'NONE',  ( 1.000000000000000000, 0.000000000000000000, 0.000000000000000000 ) ) ;
#2616 = CARTESIAN_POINT ( 'NONE',  ( 0.000000000000000000, 0.000000000000000000, 12.00000000000000000 ) ) ;
#2617 = CARTESIAN_POINT ( 'NONE',  ( 0.000000000000000000, 25.00000000000000000, 281.0000000000000000 ) ) ;
#2618 = CARTESIAN_POINT ( 'NONE',  ( -17.00000000000000000, 0.000000000000000000, -175.0000000000000000 ) ) ;
#2619 = CARTESIAN_POINT ( 'NONE',  ( 3.122849337825746672E-15, 17.00000000000000000, -20.00000000000000000 ) ) ;
#2620 = ORIENTED_EDGE ( 'NONE', *, *, #6018, .T. ) ;
#2621 = CIRCLE ( 'NONE', #3241, 46.00000000000000000 ) ;
#2622 = AXIS2_PLACEMENT_3D ( 'NONE', #4723, #4235, #2304 ) ;
#2623 = APPLICATION_PROTOCOL_DEFINITION ( 'draft international standard', 'automotive_design', 1998, #4351 ) ;
#2624 = CARTESIAN_POINT ( 'NONE',  ( -0.6825543444542548910, -20.00000000000000000, 39.27501000028010480 ) ) ;
#2625 = ADVANCED_FACE ( 'NONE', ( #5831, #457 ), #3927, .T. ) ;
#2626 = ORIENTED_EDGE ( 'NONE', *, *, #2673, .T. ) ;
#2627 = FACE_OUTER_BOUND ( 'NONE', #2071, .T. ) ;
#2628 = ORIENTED_EDGE ( 'NONE', *, *, #1060, .T. ) ;
#2629 = AXIS2_PLACEMENT_3D ( 'NONE', #437, #1429, #5372 ) ;
#2630 = VECTOR ( 'NONE', #1279, 1000.000000000000000 ) ;
#2631 = DIRECTION ( 'NONE',  ( 1.000000000000000000, 0.000000000000000000, 0.000000000000000000 ) ) ;
#2632 = CARTESIAN_POINT ( 'NONE',  ( 25.00000000000000000, 3.061616997868383043E-15, 44.00000000000000711 ) ) ;
#2633 = DIRECTION ( 'NONE',  ( 0.000000000000000000, 0.000000000000000000, 1.000000000000000000 ) ) ;
#2634 = FACE_OUTER_BOUND ( 'NONE', #1530, .T. ) ;
#2635 = VERTEX_POINT ( 'NONE', #522 ) ;
#2636 = FILL_AREA_STYLE_COLOUR ( '', #2045 ) ;
#2637 = FILL_AREA_STYLE ('',( #4537 ) ) ;
#2638 = CARTESIAN_POINT ( 'NONE',  ( 6.011784583892834100, 22.20189362571451142, 36.28151155367954317 ) ) ;
#2639 = AXIS2_PLACEMENT_3D ( 'NONE', #4356, #1784, #3756 ) ;
#2640 = CARTESIAN_POINT ( 'NONE',  ( -10.99369682877389209, 22.46365890119679065, 6.219949983291193085 ) ) ;
#2641 = FACE_OUTER_BOUND ( 'NONE', #6287, .T. ) ;
#2642 = ORIENTED_EDGE ( 'NONE', *, *, #2662, .T. ) ;
#2643 = EDGE_LOOP ( 'NONE', ( #4329, #5714, #1370, #4459 ) ) ;
#2644 = ORIENTED_EDGE ( 'NONE', *, *, #2353, .F. ) ;
#2645 = AXIS2_PLACEMENT_3D ( 'NONE', #3290, #5230, #4803 ) ;
#2646 = CARTESIAN_POINT ( 'NONE',  ( 0.000000000000000000, 0.000000000000000000, 39.00000000000001421 ) ) ;
#2647 = CARTESIAN_POINT ( 'NONE',  ( 22.21770253897382474, 3.871672004622519037, -175.0000000000000284 ) ) ;
#2648 = DIRECTION ( 'NONE',  ( 1.000000000000000000, 0.000000000000000000, 0.000000000000000000 ) ) ;
#2649 = VECTOR ( 'NONE', #1387, 1000.000000000000000 ) ;
#2650 = CARTESIAN_POINT ( 'NONE',  ( 0.000000000000000000, 25.00000000000000000, -195.0000000000000000 ) ) ;
#2651 = DIRECTION ( 'NONE',  ( 1.000000000000000000, 0.000000000000000000, 0.000000000000000000 ) ) ;
#2652 = ORIENTED_EDGE ( 'NONE', *, *, #390, .T. ) ;
#2653 = EDGE_CURVE ( 'NONE', #2747, #1338, #4269, .T. ) ;
#2654 = DIRECTION ( 'NONE',  ( 0.000000000000000000, 0.000000000000000000, -1.000000000000000000 ) ) ;
#2655 = DIRECTION ( 'NONE',  ( 0.000000000000000000, -1.000000000000000000, 1.740526192617802767E-17 ) ) ;
#2656 = EDGE_CURVE ( 'NONE', #990, #3225, #3167, .T. ) ;
#2657 = ORIENTED_EDGE ( 'NONE', *, *, #3608, .F. ) ;
#2658 = AXIS2_PLACEMENT_3D ( 'NONE', #384, #2305, #5284 ) ;
#2659 = PRODUCT_DEFINITION_SHAPE ( 'NONE', 'NONE',  #1341 ) ;
#2660 = DIRECTION ( 'NONE',  ( 0.000000000000000000, 1.000000000000000000, 0.000000000000000000 ) ) ;
#2661 = ORIENTED_EDGE ( 'NONE', *, *, #3013, .T. ) ;
#2662 = EDGE_CURVE ( 'NONE', #2995, #686, #5142, .T. ) ;
#2663 = AXIS2_PLACEMENT_3D ( 'NONE', #4944, #3550, #4513 ) ;
#2664 = DIRECTION ( 'NONE',  ( -0.000000000000000000, -0.000000000000000000, -1.000000000000000000 ) ) ;
#2665 = DIRECTION ( 'NONE',  ( 1.000000000000000000, 0.000000000000000000, -0.000000000000000000 ) ) ;
#2666 = DIRECTION ( 'NONE',  ( 0.000000000000000000, 0.000000000000000000, 1.000000000000000000 ) ) ;
#2667 = AXIS2_PLACEMENT_3D ( 'NONE', #1062, #3938, #3901 ) ;
#2668 = DIRECTION ( 'NONE',  ( -0.000000000000000000, -0.000000000000000000, -1.000000000000000000 ) ) ;
#2669 = ORIENTED_EDGE ( 'NONE', *, *, #5541, .F. ) ;
#2670 = DIRECTION ( 'NONE',  ( 1.224646799147353207E-16, 1.000000000000000000, -0.000000000000000000 ) ) ;
#2671 = CARTESIAN_POINT ( 'NONE',  ( 12.50000000000000355, 120.0000000000000000, 12.00000000000000000 ) ) ;
#2672 = CYLINDRICAL_SURFACE ( 'NONE', #4973, 90.00000000000322586 ) ;
#2673 = EDGE_CURVE ( 'NONE', #4815, #6280, #4204, .T. ) ;
#2674 = CARTESIAN_POINT ( 'NONE',  ( -8.266016972479206970, 23.60732501453303200, 7.985288904279078892 ) ) ;
#2675 = CIRCLE ( 'NONE', #6289, 22.67164836619070911 ) ;
#2676 = CARTESIAN_POINT ( 'NONE',  ( -17.05141243254543681, -12.25762350764760455, 0.000000000000000000 ) ) ;
#2677 = VERTEX_POINT ( 'NONE', #6170 ) ;
#2678 = ORIENTED_EDGE ( 'NONE', *, *, #2401, .F. ) ;
#2679 = DIRECTION ( 'NONE',  ( 1.000000000000000000, 0.000000000000000000, 0.000000000000000000 ) ) ;
#2680 = LINE ( 'NONE', #5175, #894 ) ;
#2681 = DIRECTION ( 'NONE',  ( 0.000000000000000000, 0.000000000000000000, 1.000000000000000000 ) ) ;
#2682 = DIRECTION ( 'NONE',  ( 0.000000000000000000, -1.000000000000000000, 0.000000000000000000 ) ) ;
#2683 = CIRCLE ( 'NONE', #2485, 25.00000000000000000 ) ;
#2684 = CARTESIAN_POINT ( 'NONE',  ( -2.385244779468109755E-15, -1.040834085586084257E-14, -130.0000000000000000 ) ) ;
#2685 = ORIENTED_EDGE ( 'NONE', *, *, #548, .F. ) ;
#2686 = DIRECTION ( 'NONE',  ( -0.000000000000000000, -0.000000000000000000, -1.000000000000000000 ) ) ;
#2687 = CARTESIAN_POINT ( 'NONE',  ( 12.24406280880444164, -19.48300239097275721, 5.141666792244760309 ) ) ;
#2688 = ORIENTED_EDGE ( 'NONE', *, *, #1126, .T. ) ;
#2689 = LINE ( 'NONE', #5501, #1547 ) ;
#2690 = ORIENTED_EDGE ( 'NONE', *, *, #2272, .T. ) ;
#2691 = CARTESIAN_POINT ( 'NONE',  ( 0.000000000000000000, 25.00000000000000000, -195.0000000000000000 ) ) ;
#2692 = UNCERTAINTY_MEASURE_WITH_UNIT (LENGTH_MEASURE( 1.000000000000000082E-05 ), #5255, 'distance_accuracy_value', 'NONE');
#2693 = LINE ( 'NONE', #2796, #4333 ) ;
#2694 = FACE_OUTER_BOUND ( 'NONE', #4001, .T. ) ;
#2695 = FACE_OUTER_BOUND ( 'NONE', #5882, .T. ) ;
#2696 = VERTEX_POINT ( 'NONE', #1658 ) ;
#2697 = FACE_OUTER_BOUND ( 'NONE', #6143, .T. ) ;
#2698 = EDGE_LOOP ( 'NONE', ( #4968, #4895, #885, #1499 ) ) ;
#2699 = FACE_OUTER_BOUND ( 'NONE', #1859, .T. ) ;
#2700 = DIRECTION ( 'NONE',  ( -0.000000000000000000, -0.000000000000000000, -1.000000000000000000 ) ) ;
#2701 = CARTESIAN_POINT ( 'NONE',  ( -1.764366888834147495, 24.94145795391612808, 9.917654830493177087 ) ) ;
#2702 = FACE_OUTER_BOUND ( 'NONE', #277, .T. ) ;
#2703 = EDGE_LOOP ( 'NONE', ( #2908, #326, #5490, #5307 ) ) ;
#2704 = ORIENTED_EDGE ( 'NONE', *, *, #5614, .F. ) ;
#2705 = CARTESIAN_POINT ( 'NONE',  ( -5.958341177435922731, 24.28123298992124290, 27.19342269918142563 ) ) ;
#2706 = PRODUCT_DEFINITION_SHAPE ( 'NONE', 'NONE',  #6372 ) ;
#2707 = FACE_OUTER_BOUND ( 'NONE', #4912, .T. ) ;
#2708 = DIRECTION ( 'NONE',  ( -0.000000000000000000, -0.000000000000000000, -1.000000000000000000 ) ) ;
#2709 = CARTESIAN_POINT ( 'NONE',  ( 17.00000000000000000, 0.000000000000000000, -49.99999999999999289 ) ) ;
#2710 = ORIENTED_EDGE ( 'NONE', *, *, #4153, .T. ) ;
#2711 = LINE ( 'NONE', #6138, #2748 ) ;
#2712 = ORIENTED_EDGE ( 'NONE', *, *, #390, .F. ) ;
#2713 = DIRECTION ( 'NONE',  ( -1.000000000000000000, 0.000000000000000000, 0.000000000000000000 ) ) ;
#2714 = CARTESIAN_POINT ( 'NONE',  ( 8.270741877429188094, -21.47680860501242961, 7.983294599549966897 ) ) ;
#2715 = EDGE_LOOP ( 'NONE', ( #1986, #3776, #3494, #4205, #3644, #2306, #1177 ) ) ;
#2716 = DIRECTION ( 'NONE',  ( 0.000000000000000000, 0.000000000000000000, 1.000000000000000000 ) ) ;
#2717 = ORIENTED_EDGE ( 'NONE', *, *, #3933, .T. ) ;
#2718 = CIRCLE ( 'NONE', #3553, 6.500000000000000000 ) ;
#2719 = DIRECTION ( 'NONE',  ( 1.000000000000000000, 0.000000000000000000, 0.000000000000000000 ) ) ;
#2720 = FACE_BOUND ( 'NONE', #618, .T. ) ;
#2721 = EDGE_CURVE ( 'NONE', #5017, #4627, #3490, .T. ) ;
#2722 = CYLINDRICAL_SURFACE ( 'NONE', #3478, 46.00000000000000000 ) ;
#2723 = DIRECTION ( 'NONE',  ( -0.000000000000000000, -0.000000000000000000, -1.000000000000000000 ) ) ;
#2724 = ORIENTED_EDGE ( 'NONE', *, *, #5756, .F. ) ;
#2725 = CARTESIAN_POINT ( 'NONE',  ( 0.000000000000000000, 120.0000000000000000, 12.00000000000000000 ) ) ;
#2726 = ORIENTED_EDGE ( 'NONE', *, *, #3994, .T. ) ;
#2727 = CARTESIAN_POINT ( 'NONE',  ( 7.487557334333944326, 23.85240338065036880, 32.27275042597646149 ) ) ;
#2728 = FACE_OUTER_BOUND ( 'NONE', #2200, .T. ) ;
#2729 = ADVANCED_FACE ( 'NONE', ( #314, #4193 ), #1236, .T. ) ;
#2730 = ADVANCED_FACE ( 'NONE', ( #736 ), #219, .F. ) ;
#2731 = DIRECTION ( 'NONE',  ( 1.000000000000000000, 0.000000000000000000, 0.000000000000000000 ) ) ;
#2732 = CIRCLE ( 'NONE', #3162, 14.00000000000000000 ) ;
#2734 = EDGE_CURVE ( 'NONE', #5912, #3044, #1199, .T. ) ;
#2733 = LINE ( 'NONE', #5552, #5143 ) ;
#2735 = ORIENTED_EDGE ( 'NONE', *, *, #1457, .T. ) ;
#2736 = ORIENTED_EDGE ( 'NONE', *, *, #1647, .F. ) ;
#2737 = CARTESIAN_POINT ( 'NONE',  ( -7.500225230914492336, 23.84840920358613303, 32.26396939133217501 ) ) ;
#2738 = ADVANCED_FACE ( 'NONE', ( #4156, #3683 ), #6134, .F. ) ;
#2739 = EDGE_CURVE ( 'NONE', #3765, #6038, #209, .T. ) ;
#2740 = AXIS2_PLACEMENT_3D ( 'NONE', #844, #360, #2314 ) ;
#2741 = CARTESIAN_POINT ( 'NONE',  ( 0.000000000000000000, 0.000000000000000000, 23.77500997278103512 ) ) ;
#2742 = CARTESIAN_POINT ( 'NONE',  ( 0.000000000000000000, 0.000000000000000000, 23.00000000000000000 ) ) ;
#2743 = CARTESIAN_POINT ( 'NONE',  ( 0.000000000000000000, 120.0000000000000000, 12.00000000000000000 ) ) ;
#2744 = VECTOR ( 'NONE', #6293, 1000.000000000000000 ) ;
#2745 = ORIENTED_EDGE ( 'NONE', *, *, #5272, .T. ) ;
#2746 = DIRECTION ( 'NONE',  ( -1.000000000000000000, 0.000000000000000000, 0.000000000000000000 ) ) ;
#2747 = VERTEX_POINT ( 'NONE', #2709 ) ;
#2748 = VECTOR ( 'NONE', #4685, 1000.000000000000000 ) ;
#2749 = CARTESIAN_POINT ( 'NONE',  ( -7.200995294576264527, -21.84734027758491237, 8.482870732638906119 ) ) ;
#2750 = VERTEX_POINT ( 'NONE', #4681 ) ;
#2751 = CARTESIAN_POINT ( 'NONE',  ( -13.14183123006980480, 39.58265509608657595, -45.00000000000000000 ) ) ;
#2752 = ORIENTED_EDGE ( 'NONE', *, *, #1232, .T. ) ;
#2753 = FILL_AREA_STYLE ('',( #357 ) ) ;
#2754 =( NAMED_UNIT ( * ) PLANE_ANGLE_UNIT ( ) SI_UNIT ( $, .RADIAN. ) );
#2755 = CARTESIAN_POINT ( 'NONE',  ( 0.000000000000000000, -24.25762350764758679, 0.000000000000000000 ) ) ;
#2756 = VECTOR ( 'NONE', #547, 1000.000000000000000 ) ;
#2757 = DIRECTION ( 'NONE',  ( 1.000000000000000000, 0.000000000000000000, 0.000000000000000000 ) ) ;
#2758 = CARTESIAN_POINT ( 'NONE',  ( 3.122849337825746672E-15, 17.00000000000000000, 281.0000000000000000 ) ) ;
#2759 = ORIENTED_EDGE ( 'NONE', *, *, #5833, .F. ) ;
#2760 = CARTESIAN_POINT ( 'NONE',  ( 16.00000000000000355, 1.959434878635765526E-15, 16.00000000000000000 ) ) ;
#2762 = ORIENTED_EDGE ( 'NONE', *, *, #4874, .F. ) ;
#2761 = VECTOR ( 'NONE', #1336, 1000.000000000000000 ) ;
#2763 = EDGE_CURVE ( 'NONE', #5556, #1537, #2229, .T. ) ;
#2764 = DIRECTION ( 'NONE',  ( 0.000000000000000000, -1.000000000000000000, 0.000000000000000000 ) ) ;
#2765 = CARTESIAN_POINT ( 'NONE',  ( -17.00000000000000355, -25.00000000000000000, -130.0000000000000000 ) ) ;
#2766 = CIRCLE ( 'NONE', #5360, 17.00000000000000000 ) ;
#2767 = DIRECTION ( 'NONE',  ( -1.000000000000000000, -0.000000000000000000, -0.000000000000000000 ) ) ;
#2768 = CARTESIAN_POINT ( 'NONE',  ( 7.115105366545459553, -23.96693872413611004, 34.19760250332532081 ) ) ;
#2769 = EDGE_CURVE ( 'NONE', #5038, #3626, #3723, .T. ) ;
#2770 = ORIENTED_EDGE ( 'NONE', *, *, #2203, .T. ) ;
#2771 = EDGE_LOOP ( 'NONE', ( #3292, #1471, #1818, #2308 ) ) ;
#2772 = CIRCLE ( 'NONE', #6285, 1.000000000000000000 ) ;
#2773 = CARTESIAN_POINT ( 'NONE',  ( -5.951225761847359408, 24.28185285436555674, 36.34586759703542214 ) ) ;
#2774 = LINE ( 'NONE', #3784, #5110 ) ;
#2775 = CARTESIAN_POINT ( 'NONE',  ( 0.000000000000000000, 69.00000000000000000, 110.0000000000000000 ) ) ;
#2776 = EDGE_CURVE ( 'NONE', #2027, #4920, #4418, .T. ) ;
#2777 = DIRECTION ( 'NONE',  ( 1.000000000000000000, 0.000000000000000000, 0.000000000000000000 ) ) ;
#2778 = ADVANCED_FACE ( 'NONE', ( #5205 ), #795, .T. ) ;
#2779 = EDGE_LOOP ( 'NONE', ( #471, #5368, #3902, #1809 ) ) ;
#2780 = VERTEX_POINT ( 'NONE', #5563 ) ;
#2781 = AXIS2_PLACEMENT_3D ( 'NONE', #1005, #2963, #1939 ) ;
#2782 = AXIS2_PLACEMENT_3D ( 'NONE', #926, #2880, #2078 ) ;
#2783 = DIRECTION ( 'NONE',  ( -1.000000000000000000, 0.000000000000000000, 0.000000000000000000 ) ) ;
#2784 = ADVANCED_FACE ( 'NONE', ( #6107 ), #5109, .F. ) ;
#2785 = CONTEXT_DEPENDENT_SHAPE_REPRESENTATION ( #5141, #772 ) ;
#2786 = CARTESIAN_POINT ( 'NONE',  ( 6.736606839469455821, -22.00628563274161920, 8.696944893850881542 ) ) ;
#2787 = CARTESIAN_POINT ( 'NONE',  ( 0.000000000000000000, 0.000000000000000000, 51.00000000000002842 ) ) ;
#2788 = AXIS2_PLACEMENT_3D ( 'NONE', #5256, #2312, #391 ) ;
#2789 = ADVANCED_BREP_SHAPE_REPRESENTATION ( '', ( #4438, #6349 ), #5524 ) ;
#2790 = PRODUCT_DEFINITION ( 'UNKNOWN', '', #6116, #5010 ) ;
#2791 = ORIENTED_EDGE ( 'NONE', *, *, #4137, .T. ) ;
#2792 = LINE ( 'NONE', #5770, #3712 ) ;
#2793 = ORIENTED_EDGE ( 'NONE', *, *, #5278, .T. ) ;
#2794 = CARTESIAN_POINT ( 'NONE',  ( -0.2052511266214760433, -21.25619793154163517, -65.00000000000000000 ) ) ;
#2795 = EDGE_CURVE ( 'NONE', #3396, #1816, #3079, .T. ) ;
#2796 = CARTESIAN_POINT ( 'NONE',  ( 279.0000000000000000, 68.99999999999997158, 110.0000000000000000 ) ) ;
#2797 = CARTESIAN_POINT ( 'NONE',  ( -17.00000000000000000, 0.000000000000000000, 48.00000000000000000 ) ) ;
#2798 = CARTESIAN_POINT ( 'NONE',  ( -4.574685241957346271, -24.57863749249464291, 25.82670804586579294 ) ) ;
#2799 = ORIENTED_EDGE ( 'NONE', *, *, #588, .F. ) ;
#2800 = DIRECTION ( 'NONE',  ( -1.000000000000000000, 0.000000000000000000, 0.000000000000000000 ) ) ;
#2801 = EDGE_LOOP ( 'NONE', ( #5037, #2685, #5331, #3655 ) ) ;
#2802 = CARTESIAN_POINT ( 'NONE',  ( -0.3392246580399966294, 19.99999999999999645, 39.27501000028010480 ) ) ;
#2803 = DIRECTION ( 'NONE',  ( -1.000000000000000000, 0.000000000000000000, 0.000000000000000000 ) ) ;
#2804 = CARTESIAN_POINT ( 'NONE',  ( 6.500000000000000000, 130.6770782520313219, 12.00000000000000000 ) ) ;
#2805 = VECTOR ( 'NONE', #636, 1000.000000000000000 ) ;
#2806 = CARTESIAN_POINT ( 'NONE',  ( 2.436617367782499599, -22.87153588547686667, 24.67833651202806067 ) ) ;
#2807 = VERTEX_POINT ( 'NONE', #3323 ) ;
#2808 = ORIENTED_EDGE ( 'NONE', *, *, #2847, .T. ) ;
#2809 = CARTESIAN_POINT ( 'NONE',  ( -7.018581182383311301, 23.99477090726735895, 29.12000203626552164 ) ) ;
#2810 = DIRECTION ( 'NONE',  ( 0.000000000000000000, 0.000000000000000000, -1.000000000000000000 ) ) ;
#2811 = FACE_OUTER_BOUND ( 'NONE', #3128, .T. ) ;
#2812 = ADVANCED_FACE ( 'NONE', ( #5374, #5304 ), #889, .F. ) ;
#2813 = CARTESIAN_POINT ( 'NONE',  ( 9.185524248261779151E-16, 25.00000000000000000, 39.27501000028010480 ) ) ;
#2814 = ORIENTED_EDGE ( 'NONE', *, *, #1591, .F. ) ;
#2815 = EDGE_LOOP ( 'NONE', ( #2678, #2418 ) ) ;
#2816 = DIRECTION ( 'NONE',  ( -0.000000000000000000, -0.000000000000000000, 1.000000000000000000 ) ) ;
#2817 = CARTESIAN_POINT ( 'NONE',  ( -12.66240722304475774, 29.37208741619406993, 9.875474163642433467 ) ) ;
#2818 = DIRECTION ( 'NONE',  ( 1.000000000000000000, 0.000000000000000000, 0.000000000000000000 ) ) ;
#2819 = ORIENTED_EDGE ( 'NONE', *, *, #187, .F. ) ;
#2820 = DIRECTION ( 'NONE',  ( -0.000000000000000000, -0.000000000000000000, -1.000000000000000000 ) ) ;
#2821 = DIRECTION ( 'NONE',  ( 1.000000000000000000, 0.000000000000000000, 0.000000000000000000 ) ) ;
#2822 = CARTESIAN_POINT ( 'NONE',  ( -2.012341796004660122, -22.91179784512888773, 39.00000000000001421 ) ) ;
#2823 = CARTESIAN_POINT ( 'NONE',  ( -7.102515314070984687, -23.96997983984567782, 29.35314634237168718 ) ) ;
#2824 = ORIENTED_EDGE ( 'NONE', *, *, #5920, .T. ) ;
#2825 = DIRECTION ( 'NONE',  ( 0.000000000000000000, 0.000000000000000000, 1.000000000000000000 ) ) ;
#2826 = CARTESIAN_POINT ( 'NONE',  ( 6.502944117165512239, 24.14103883855864652, 35.54306285688424794 ) ) ;
#2827 = DIRECTION ( 'NONE',  ( 1.000000000000000000, 0.000000000000000000, 0.000000000000000000 ) ) ;
#2828 = VECTOR ( 'NONE', #1602, 1000.000000000000000 ) ;
#2829 = DIRECTION ( 'NONE',  ( 0.000000000000000000, 0.000000000000000000, -1.000000000000000000 ) ) ;
#2830 = CARTESIAN_POINT ( 'NONE',  ( 2.655777422895189144, -24.85958502782042601, 24.75666344040547884 ) ) ;
#2831 = VERTEX_POINT ( 'NONE', #2397 ) ;
#2832 = EDGE_LOOP ( 'NONE', ( #2256, #976, #5186, #3086 ) ) ;
#2833 = FACE_OUTER_BOUND ( 'NONE', #52, .T. ) ;
#2834 = AXIS2_PLACEMENT_3D ( 'NONE', #4189, #3721, #763 ) ;
#2835 = CIRCLE ( 'NONE', #6244, 22.67164836619070911 ) ;
#2836 = DIRECTION ( 'NONE',  ( -0.000000000000000000, -0.000000000000000000, 1.000000000000000000 ) ) ;
#2837 = VECTOR ( 'NONE', #4214, 1000.000000000000000 ) ;
#2838 = CARTESIAN_POINT ( 'NONE',  ( 0.000000000000000000, 0.000000000000000000, 0.000000000000000000 ) ) ;
#2839 = DIRECTION ( 'NONE',  ( 1.000000000000000000, 0.000000000000000000, 0.000000000000000000 ) ) ;
#2840 = EDGE_LOOP ( 'NONE', ( #780, #3751, #5763, #2561, #863, #3801 ) ) ;
#2841 = ORIENTED_EDGE ( 'NONE', *, *, #4098, .T. ) ;
#2842 = DIRECTION ( 'NONE',  ( 0.000000000000000000, 0.000000000000000000, 1.000000000000000000 ) ) ;
#2843 = CARTESIAN_POINT ( 'NONE',  ( 17.00000000000000000, 0.000000000000000000, -110.0000000000000000 ) ) ;
#2844 = AXIS2_PLACEMENT_3D ( 'NONE', #3995, #4974, #2493 ) ;
#2845 = LINE ( 'NONE', #3733, #2881 ) ;
#2846 = ORIENTED_EDGE ( 'NONE', *, *, #6209, .T. ) ;
#2847 = EDGE_CURVE ( 'NONE', #5271, #1144, #412, .T. ) ;
#2848 = EDGE_CURVE ( 'NONE', #861, #5038, #5033, .T. ) ;
#2849 = AXIS2_PLACEMENT_3D ( 'NONE', #3899, #5878, #3182 ) ;
#2850 = DIRECTION ( 'NONE',  ( -0.000000000000000000, -0.000000000000000000, -1.000000000000000000 ) ) ;
#2851 = CARTESIAN_POINT ( 'NONE',  ( -2.226229255992760780, -22.89589894665499870, 24.59902000234163211 ) ) ;
#2852 = CARTESIAN_POINT ( 'NONE',  ( 0.000000000000000000, 76.99999716619419132, 281.0000000000000000 ) ) ;
#2853 = AXIS2_PLACEMENT_3D ( 'NONE', #3503, #3469, #3853 ) ;
#2854 = DIRECTION ( 'NONE',  ( -0.000000000000000000, -0.000000000000000000, -1.000000000000000000 ) ) ;
#2855 = VERTEX_POINT ( 'NONE', #4357 ) ;
#2856 = EDGE_CURVE ( 'NONE', #1773, #6074, #3786, .T. ) ;
#2857 = DIRECTION ( 'NONE',  ( 1.000000000000000000, 0.000000000000000000, 0.000000000000000000 ) ) ;
#2858 = CARTESIAN_POINT ( 'NONE',  ( 3.337067332043157197, 24.78046181229916911, 25.04046888573288498 ) ) ;
#2859 = EDGE_CURVE ( 'NONE', #4159, #1293, #6165, .T. ) ;
#2860 = DIRECTION ( 'NONE',  ( 0.000000000000000000, -1.000000000000000000, 0.000000000000000000 ) ) ;
#2861 = AXIS2_PLACEMENT_3D ( 'NONE', #859, #4813, #4849 ) ;
#2862 = CARTESIAN_POINT ( 'NONE',  ( 4.600626795032661143, -22.53777557106161922, 25.83521031145350122 ) ) ;
#2863 = ORIENTED_EDGE ( 'NONE', *, *, #3610, .T. ) ;
#2864 = PRODUCT_DEFINITION ( 'UNKNOWN', '', #3754, #1316 ) ;
#2865 = VECTOR ( 'NONE', #3077, 1000.000000000000000 ) ;
#2866 = DIRECTION ( 'NONE',  ( 0.000000000000000000, 0.000000000000000000, -1.000000000000000000 ) ) ;
#2867 = EDGE_CURVE ( 'NONE', #157, #5299, #5867, .T. ) ;
#2868 = ORIENTED_EDGE ( 'NONE', *, *, #3538, .F. ) ;
#2869 = CARTESIAN_POINT ( 'NONE',  ( -4.050825139678606135, 22.64130375691644304, 38.09092692957536030 ) ) ;
#2870 = EDGE_CURVE ( 'NONE', #554, #3333, #3900, .T. ) ;
#2871 = VECTOR ( 'NONE', #685, 1000.000000000000000 ) ;
#2872 = ADVANCED_FACE ( 'NONE', ( #5819 ), #1888, .F. ) ;
#2873 = CARTESIAN_POINT ( 'NONE',  ( -6.500000000000000000, 130.6770782520313219, 12.00000000000000000 ) ) ;
#2874 = FACE_OUTER_BOUND ( 'NONE', #4752, .T. ) ;
#2875 = CARTESIAN_POINT ( 'NONE',  ( 279.0000000000000000, 14.00000000000000000, 110.0000000000000000 ) ) ;
#2876 = VERTEX_POINT ( 'NONE', #2875 ) ;
#2877 = ORIENTED_EDGE ( 'NONE', *, *, #2271, .T. ) ;
#2878 = ORIENTED_EDGE ( 'NONE', *, *, #1048, .F. ) ;
#2879 = VECTOR ( 'NONE', #3992, 1000.000000000000000 ) ;
#2880 = DIRECTION ( 'NONE',  ( -0.000000000000000000, -0.000000000000000000, -1.000000000000000000 ) ) ;
#2881 = VECTOR ( 'NONE', #4163, 1000.000000000000000 ) ;
#2882 = CARTESIAN_POINT ( 'NONE',  ( 22.21770253897382474, 3.871672004622519037, -130.0000000000000000 ) ) ;
#2883 = AXIS2_PLACEMENT_3D ( 'NONE', #4220, #2319, #1319 ) ;
#2884 = CIRCLE ( 'NONE', #2373, 16.00000000000000355 ) ;
#2885 = CARTESIAN_POINT ( 'NONE',  ( -4.258741324358278568, -24.63828325354172222, 9.488137494773077663 ) ) ;
#2886 = EDGE_LOOP ( 'NONE', ( #3789, #171, #4841, #4850 ) ) ;
#2887 = DIRECTION ( 'NONE',  ( -0.000000000000000000, 0.000000000000000000, 1.000000000000000000 ) ) ;
#2888 = CARTESIAN_POINT ( 'NONE',  ( -163.6881948289521347, 13.87638965790611500, 224.0000000000000284 ) ) ;
#2889 = CARTESIAN_POINT ( 'NONE',  ( 0.000000000000000000, 0.000000000000000000, 12.00000000000000000 ) ) ;
#2890 = CARTESIAN_POINT ( 'NONE',  ( 59.99991398172927859, 76.99999716619419132, 276.0000000000000000 ) ) ;
#2891 = DIRECTION ( 'NONE',  ( 0.000000000000000000, -0.000000000000000000, 1.000000000000000000 ) ) ;
#2892 = ORIENTED_EDGE ( 'NONE', *, *, #358, .F. ) ;
#2893 =( NAMED_UNIT ( * ) SI_UNIT ( $, .STERADIAN. ) SOLID_ANGLE_UNIT ( ) );
#2894 = AXIS2_PLACEMENT_3D ( 'NONE', #199, #1981, #4109 ) ;
#2895 = DIRECTION ( 'NONE',  ( -1.000000000000000000, 0.000000000000000000, 0.000000000000000000 ) ) ;
#2896 = DIRECTION ( 'NONE',  ( -1.000000000000000000, 0.000000000000000000, 0.000000000000000000 ) ) ;
#2897 = FACE_OUTER_BOUND ( 'NONE', #6030, .T. ) ;
#2898 = VERTEX_POINT ( 'NONE', #1915 ) ;
#2899 = LINE ( 'NONE', #318, #6263 ) ;
#2900 = ORIENTED_EDGE ( 'NONE', *, *, #4751, .T. ) ;
#2901 = CARTESIAN_POINT ( 'NONE',  ( -17.05141243254543681, -24.25762350764758679, 12.00000000000000000 ) ) ;
#2902 = CYLINDRICAL_SURFACE ( 'NONE', #5001, 16.00000000000000000 ) ;
#2903 = CIRCLE ( 'NONE', #3945, 17.00000000000000000 ) ;
#2904 = CARTESIAN_POINT ( 'NONE',  ( -0.2052511266214760433, -21.25619793154163517, -110.0000000000000000 ) ) ;
#2905 = DIRECTION ( 'NONE',  ( 1.000000000000000000, 0.000000000000000000, 0.000000000000000000 ) ) ;
#2906 = VERTEX_POINT ( 'NONE', #1396 ) ;
#2907 = ORIENTED_EDGE ( 'NONE', *, *, #1326, .T. ) ;
#2908 = ORIENTED_EDGE ( 'NONE', *, *, #5625, .F. ) ;
#2909 = VERTEX_POINT ( 'NONE', #439 ) ;
#2910 = DIRECTION ( 'NONE',  ( 1.000000000000000000, 0.000000000000000000, 0.000000000000000000 ) ) ;
#2911 = APPLICATION_CONTEXT ( 'automotive_design' ) ;
#2912 = CARTESIAN_POINT ( 'NONE',  ( -25.00000000000000000, 0.000000000000000000, 44.00000000000000711 ) ) ;
#2913 = CARTESIAN_POINT ( 'NONE',  ( 4.322439664174057228, -24.63752030717468600, 9.487820034421874382 ) ) ;
#2914 = ORIENTED_EDGE ( 'NONE', *, *, #1406, .F. ) ;
#2915 = FACE_OUTER_BOUND ( 'NONE', #604, .T. ) ;
#2916 = PLANE ( 'NONE',  #3768 ) ;
#2917 = DIRECTION ( 'NONE',  ( -0.000000000000000000, -0.000000000000000000, -1.000000000000000000 ) ) ;
#2918 = CARTESIAN_POINT ( 'NONE',  ( 44.56092774862622719, -29.44644455561813956, 15.00000000000000000 ) ) ;
#2919 = ORIENTED_EDGE ( 'NONE', *, *, #2123, .T. ) ;
#2920 = DIRECTION ( 'NONE',  ( 0.000000000000000000, -1.000000000000000000, 0.000000000000000000 ) ) ;
#2921 = DIRECTION ( 'NONE',  ( -1.000000000000000000, 0.000000000000000000, 0.000000000000000000 ) ) ;
#2922 = DIRECTION ( 'NONE',  ( -1.000000000000000000, 0.000000000000000000, 0.000000000000000000 ) ) ;
#2923 = EDGE_CURVE ( 'NONE', #542, #5184, #4621, .T. ) ;
#2924 = LINE ( 'NONE', #3445, #2342 ) ;
#2925 = CARTESIAN_POINT ( 'NONE',  ( 0.000000000000000000, 0.000000000000000000, 23.77500997278103512 ) ) ;
#2926 = VERTEX_POINT ( 'NONE', #5853 ) ;
#2927 = CARTESIAN_POINT ( 'NONE',  ( 6.810998761473115337, 21.97232263399875762, 8.650160397932937784 ) ) ;
#2928 = ORIENTED_EDGE ( 'NONE', *, *, #6023, .F. ) ;
#2929 = CIRCLE ( 'NONE', #4892, 90.00000000000319744 ) ;
#2930 = CYLINDRICAL_SURFACE ( 'NONE', #5181, 166.8359700257217071 ) ;
#2931 = EDGE_CURVE ( 'NONE', #3745, #1293, #4877, .T. ) ;
#2932 = TOROIDAL_SURFACE ( 'NONE', #2018, 6.500000000000000000, 1.000000000000000000 ) ;
#2933 = ADVANCED_BREP_SHAPE_REPRESENTATION ( '', ( #4588, #6349 ), #389 ) ;
#2934 = EDGE_CURVE ( 'NONE', #1518, #6319, #4750, .T. ) ;
#2935 = DIRECTION ( 'NONE',  ( -1.000000000000000000, 0.000000000000000000, 0.000000000000000000 ) ) ;
#2936 = EDGE_CURVE ( 'NONE', #4613, #542, #6362, .T. ) ;
#2937 = PLANE ( 'NONE',  #3787 ) ;
#2938 = DIRECTION ( 'NONE',  ( -0.000000000000000000, -0.000000000000000000, -1.000000000000000000 ) ) ;
#2939 = EDGE_LOOP ( 'NONE', ( #88, #2400, #447, #3377 ) ) ;
#2940 = VERTEX_POINT ( 'NONE', #2813 ) ;
#2941 = ORIENTED_EDGE ( 'NONE', *, *, #5990, .F. ) ;
#2942 = ADVANCED_FACE ( 'NONE', ( #346 ), #2297, .T. ) ;
#2943 = ADVANCED_FACE ( 'NONE', ( #6238 ), #1823, .F. ) ;
#2944 = CIRCLE ( 'NONE', #4487, 22.67164836619067714 ) ;
#2945 = ORIENTED_EDGE ( 'NONE', *, *, #4656, .F. ) ;
#2946 = CARTESIAN_POINT ( 'NONE',  ( -19.00000000000000000, 2.326828918379970970E-15, -248.0000000000000000 ) ) ;
#2947 = LINE ( 'NONE', #5108, #2359 ) ;
#2948 = AXIS2_PLACEMENT_3D ( 'NONE', #126, #4338, #1623 ) ;
#2949 = CARTESIAN_POINT ( 'NONE',  ( 15.63375151319037037, -19.51424150167564875, 0.7397720130343804490 ) ) ;
#2950 = ORIENTED_EDGE ( 'NONE', *, *, #4355, .T. ) ;
#2951 = ADVANCED_FACE ( 'NONE', ( #4391 ), #5279, .T. ) ;
#2952 = CONTEXT_DEPENDENT_SHAPE_REPRESENTATION ( #502, #2706 ) ;
#2953 = DIRECTION ( 'NONE',  ( -0.000000000000000000, -0.000000000000000000, 1.000000000000000000 ) ) ;
#2954 = AXIS2_PLACEMENT_3D ( 'NONE', #1628, #2991, #3593 ) ;
#2955 = DIRECTION ( 'NONE',  ( 1.000000000000000000, 0.000000000000000000, 0.000000000000000000 ) ) ;
#2956 = CARTESIAN_POINT ( 'NONE',  ( -8.000000000000003553, 100.3953136438507272, 1.999999999999998224 ) ) ;
#2957 = DIRECTION ( 'NONE',  ( 0.000000000000000000, 0.000000000000000000, 1.000000000000000000 ) ) ;
#2958 = CARTESIAN_POINT ( 'NONE',  ( 44.56092774862622719, -29.44644455561813956, -240.0000000000000000 ) ) ;
#2959 = ORIENTED_EDGE ( 'NONE', *, *, #5989, .F. ) ;
#2960 = LINE ( 'NONE', #4929, #5765 ) ;
#2961 = VECTOR ( 'NONE', #2767, 1000.000000000000000 ) ;
#2962 = CYLINDRICAL_SURFACE ( 'NONE', #4371, 22.00000000000000000 ) ;
#2963 = DIRECTION ( 'NONE',  ( 0.000000000000000000, 0.000000000000000000, 1.000000000000000000 ) ) ;
#2964 = AXIS2_PLACEMENT_3D ( 'NONE', #3559, #4006, #2651 ) ;
#2965 = CARTESIAN_POINT ( 'NONE',  ( -12.47907056128239311, 30.13454381782201352, 1.999999999999989564 ) ) ;
#2966 = DIRECTION ( 'NONE',  ( 0.000000000000000000, -1.000000000000000000, 0.000000000000000000 ) ) ;
#2967 = ORIENTED_EDGE ( 'NONE', *, *, #2280, .F. ) ;
#2968 = ADVANCED_FACE ( 'NONE', ( #3910 ), #3423, .T. ) ;
#2969 = DIRECTION ( 'NONE',  ( 0.000000000000000000, 1.000000000000000000, -1.740526192617802767E-17 ) ) ;
#2970 = ORIENTED_EDGE ( 'NONE', *, *, #3936, .T. ) ;
#2971 = CARTESIAN_POINT ( 'NONE',  ( 0.000000000000000000, 25.00000000000000000, 0.000000000000000000 ) ) ;
#2972 = LINE ( 'NONE', #48, #5678 ) ;
#2973 = EDGE_CURVE ( 'NONE', #2143, #4017, #1332, .T. ) ;
#2974 = DIRECTION ( 'NONE',  ( 0.000000000000000000, -0.000000000000000000, 1.000000000000000000 ) ) ;
#2975 = AXIS2_PLACEMENT_3D ( 'NONE', #55, #1957, #3953 ) ;
#2976 = DIRECTION ( 'NONE',  ( -2.295390878742131754E-32, 1.239088197126290570E-16, -1.000000000000000000 ) ) ;
#2977 = ORIENTED_EDGE ( 'NONE', *, *, #6307, .F. ) ;
#2978 = ORIENTED_EDGE ( 'NONE', *, *, #4013, .F. ) ;
#2979 = ORIENTED_EDGE ( 'NONE', *, *, #875, .T. ) ;
#2980 = ORIENTED_EDGE ( 'NONE', *, *, #860, .T. ) ;
#2981 = VECTOR ( 'NONE', #3493, 1000.000000000000000 ) ;
#2982 = EDGE_CURVE ( 'NONE', #2206, #5509, #5768, .T. ) ;
#2983 = CARTESIAN_POINT ( 'NONE',  ( -6.500000000000000000, 8.572527594031472204E-16, 48.00000000000000000 ) ) ;
#2984 = DIRECTION ( 'NONE',  ( 0.000000000000000000, 0.000000000000000000, -1.000000000000000000 ) ) ;
#2985 = AXIS2_PLACEMENT_3D ( 'NONE', #4139, #3184, #1738 ) ;
#2986 = CARTESIAN_POINT ( 'NONE',  ( 0.8953912278517150991, -24.98774879684975403, 9.982794782258027411 ) ) ;
#2987 = ORIENTED_EDGE ( 'NONE', *, *, #582, .F. ) ;
#2988 = ITEM_DEFINED_TRANSFORMATION ( 'NONE', 'NONE', #2436,  #6349 ) ;
#2989 = AXIS2_PLACEMENT_3D ( 'NONE', #2958, #4497, #94 ) ;
#2990 = CARTESIAN_POINT ( 'NONE',  ( 0.000000000000000000, 0.000000000000000000, -240.0000000000000000 ) ) ;
#2991 = DIRECTION ( 'NONE',  ( -1.000000000000000000, -3.568357447239288307E-17, -3.030207807290445400E-18 ) ) ;
#2992 = CARTESIAN_POINT ( 'NONE',  ( -17.05141243254543681, 0.000000000000000000, 0.000000000000000000 ) ) ;
#2993 = DIRECTION ( 'NONE',  ( 0.000000000000000000, 1.000000000000000000, 0.000000000000000000 ) ) ;
#2994 = ORIENTED_EDGE ( 'NONE', *, *, #230, .F. ) ;
#2995 = VERTEX_POINT ( 'NONE', #4456 ) ;
#2996 = CYLINDRICAL_SURFACE ( 'NONE', #1945, 4.000000000000003553 ) ;
#2997 = ORIENTED_EDGE ( 'NONE', *, *, #1626, .F. ) ;
#2998 = EDGE_CURVE ( 'NONE', #4881, #1386, #5400, .T. ) ;
#2999 = DIRECTION ( 'NONE',  ( -1.000000000000000000, 0.000000000000000000, 0.000000000000000000 ) ) ;
#3000 = LINE ( 'NONE', #1006, #708 ) ;
#3001 = AXIS2_PLACEMENT_3D ( 'NONE', #4907, #505, #4426 ) ;
#3002 = PLANE ( 'NONE',  #316 ) ;
#3003 = EDGE_LOOP ( 'NONE', ( #5821, #6234 ) ) ;
#3004 = CARTESIAN_POINT ( 'NONE',  ( 13.87989846901268187, 18.35105360579683165, 3.366461006762181185 ) ) ;
#3005 = CARTESIAN_POINT ( 'NONE',  ( 12.47915588485119898, 30.13418267071338263, 9.999999999999991118 ) ) ;
#3006 = DIRECTION ( 'NONE',  ( -1.000000000000000000, 0.000000000000000000, 0.000000000000000000 ) ) ;
#3007 = DIRECTION ( 'NONE',  ( 1.000000000000000000, 0.000000000000000000, 0.000000000000000000 ) ) ;
#3008 = CARTESIAN_POINT ( 'NONE',  ( -19.25293315802951000, 8.385974291186927942, 0.000000000000000000 ) ) ;
#3009 = CARTESIAN_POINT ( 'NONE',  ( 0.000000000000000000, 0.000000000000000000, 276.0000000000000000 ) ) ;
#3010 = ORIENTED_EDGE ( 'NONE', *, *, #3131, .F. ) ;
#3011 = ORIENTED_EDGE ( 'NONE', *, *, #946, .T. ) ;
#3012 = CYLINDRICAL_SURFACE ( 'NONE', #5838, 22.67164836619066648 ) ;
#3013 = EDGE_CURVE ( 'NONE', #1273, #4284, #3457, .T. ) ;
#3014 = PLANE ( 'NONE',  #2562 ) ;
#3015 = DIRECTION ( 'NONE',  ( -1.000000000000000000, 0.000000000000000000, 0.000000000000000000 ) ) ;
#3016 = VERTEX_POINT ( 'NONE', #1069 ) ;
#3017 = EDGE_CURVE ( 'NONE', #1786, #2027, #3997, .T. ) ;
#3018 = CARTESIAN_POINT ( 'NONE',  ( -57.68819482895220574, 82.87638965790608836, 217.8450751759959019 ) ) ;
#3019 = DIRECTION ( 'NONE',  ( -0.000000000000000000, -0.000000000000000000, -1.000000000000000000 ) ) ;
#3020 = DIRECTION ( 'NONE',  ( 0.000000000000000000, 0.000000000000000000, -1.000000000000000000 ) ) ;
#3021 = ORIENTED_EDGE ( 'NONE', *, *, #5341, .T. ) ;
#3022 = CARTESIAN_POINT ( 'NONE',  ( -43.99999999999987921, 13.41640786499904969, -95.00000000000000000 ) ) ;
#3023 = ADVANCED_FACE ( 'NONE', ( #5432 ), #1527, .T. ) ;
#3024 = EDGE_CURVE ( 'NONE', #2926, #5632, #5966, .T. ) ;
#3025 = PRODUCT_DEFINITION_FORMATION_WITH_SPECIFIED_SOURCE ( 'ANY', '', #3229, .NOT_KNOWN. ) ;
#3026 = CARTESIAN_POINT ( 'NONE',  ( 0.000000000000000000, -67.50000000000001421, 5.000000000000002665 ) ) ;
#3027 = CARTESIAN_POINT ( 'NONE',  ( 0.000000000000000000, 0.000000000000000000, 50.00000000000000711 ) ) ;
#3028 = PRODUCT_DEFINITION_FORMATION_WITH_SPECIFIED_SOURCE ( 'ANY', '', #6067, .NOT_KNOWN. ) ;
#3029 = DIRECTION ( 'NONE',  ( -0.000000000000000000, -0.000000000000000000, 1.000000000000000000 ) ) ;
#3030 = ORIENTED_EDGE ( 'NONE', *, *, #3415, .T. ) ;
#3031 = DIRECTION ( 'NONE',  ( -0.000000000000000000, -0.000000000000000000, 1.000000000000000000 ) ) ;
#3032 = ORIENTED_EDGE ( 'NONE', *, *, #5227, .T. ) ;
#3033 = CARTESIAN_POINT ( 'NONE',  ( 6.802364521716127044, 21.97126452515143313, 28.60827024242000149 ) ) ;
#3034 = DIRECTION ( 'NONE',  ( -1.734723475976809855E-15, -1.000000000000000000, 0.000000000000000000 ) ) ;
#3035 = LINE ( 'NONE', #50, #1535 ) ;
#3036 = ORIENTED_EDGE ( 'NONE', *, *, #2570, .F. ) ;
#3037 = ORIENTED_EDGE ( 'NONE', *, *, #3331, .F. ) ;
#3038 = AXIS2_PLACEMENT_3D ( 'NONE', #3563, #5532, #1106 ) ;
#3039 = EDGE_LOOP ( 'NONE', ( #2583, #2057, #1510, #82 ) ) ;
#3040 = FACE_OUTER_BOUND ( 'NONE', #3237, .T. ) ;
#3041 = CARTESIAN_POINT ( 'NONE',  ( -3.061616997868383043E-15, -25.00000000000000000, -130.0000000000000000 ) ) ;
#3042 = CARTESIAN_POINT ( 'NONE',  ( 44.00000000000000000, -13.41640786499874771, 15.00000000000000000 ) ) ;
#3043 = DIRECTION ( 'NONE',  ( 1.000000000000000000, 0.000000000000000000, 0.000000000000000000 ) ) ;
#3044 = VERTEX_POINT ( 'NONE', #2494 ) ;
#3045 = EDGE_CURVE ( 'NONE', #5103, #5880, #6278, .T. ) ;
#3046 = AXIS2_PLACEMENT_3D ( 'NONE', #2196, #4154, #3265 ) ;
#3047 = EDGE_CURVE ( 'NONE', #6022, #2461, #3035, .T. ) ;
#3048 = CARTESIAN_POINT ( 'NONE',  ( 7.311805171047937257, 82.87638965790611678, 217.8450751759956745 ) ) ;
#3049 = DIRECTION ( 'NONE',  ( -0.000000000000000000, 0.000000000000000000, -1.000000000000000000 ) ) ;
#3050 = CIRCLE ( 'NONE', #5640, 25.00000000000000000 ) ;
#3051 = ADVANCED_FACE ( 'NONE', ( #1043 ), #541, .T. ) ;
#3052 = DIRECTION ( 'NONE',  ( -1.852483853906148040E-16, 1.000000000000000000, 0.000000000000000000 ) ) ;
#3053 = ORIENTED_EDGE ( 'NONE', *, *, #3958, .F. ) ;
#3054 = VERTEX_POINT ( 'NONE', #5950 ) ;
#3055 = DIRECTION ( 'NONE',  ( -1.000000000000000000, 0.000000000000000000, 0.000000000000000000 ) ) ;
#3056 = EDGE_CURVE ( 'NONE', #4602, #1294, #2356, .T. ) ;
#3057 = DIRECTION ( 'NONE',  ( 1.000000000000000000, 0.000000000000000000, 0.000000000000000000 ) ) ;
#3058 = ADVANCED_FACE ( 'NONE', ( #2581 ), #2070, .T. ) ;
#3059 = AXIS2_PLACEMENT_3D ( 'NONE', #430, #3713, #1846 ) ;
#3060 = DIRECTION ( 'NONE',  ( 1.000000000000000000, 0.000000000000000000, 0.000000000000000000 ) ) ;
#3061 = VERTEX_POINT ( 'NONE', #4428 ) ;
#3062 = CARTESIAN_POINT ( 'NONE',  ( -17.00000000000000000, 0.000000000000000000, 23.00000000000000000 ) ) ;
#3063 = SURFACE_STYLE_USAGE ( .BOTH. , #1700 ) ;
#3064 = CARTESIAN_POINT ( 'NONE',  ( 7.472848606399997706, 21.75217170649850118, 32.55500807037982725 ) ) ;
#3065 =( GEOMETRIC_REPRESENTATION_CONTEXT ( 3 ) GLOBAL_UNCERTAINTY_ASSIGNED_CONTEXT ( ( #2241 ) ) GLOBAL_UNIT_ASSIGNED_CONTEXT ( ( #3940, #535, #1065 ) ) REPRESENTATION_CONTEXT ( 'NONE', 'WORKASPACE' ) );
#3066 = EDGE_CURVE ( 'NONE', #5880, #1742, #4730, .T. ) ;
#3067 = CARTESIAN_POINT ( 'NONE',  ( 8.933863590510663144, 23.35242969744759733, 7.599770008932984489 ) ) ;
#3068 = DIRECTION ( 'NONE',  ( 0.000000000000000000, -1.000000000000000000, 0.000000000000000000 ) ) ;
#3069 = CIRCLE ( 'NONE', #302, 17.00000000000000000 ) ;
#3070 = ORIENTED_EDGE ( 'NONE', *, *, #3608, .T. ) ;
#3071 = ORIENTED_EDGE ( 'NONE', *, *, #5756, .T. ) ;
#3072 = EDGE_LOOP ( 'NONE', ( #4855, #4658, #1442, #5857 ) ) ;
#3073 = CYLINDRICAL_SURFACE ( 'NONE', #1989, 17.00000000000000000 ) ;
#3074 = EDGE_CURVE ( 'NONE', #336, #5800, #5772, .T. ) ;
#3075 = CIRCLE ( 'NONE', #4720, 19.00000000000000000 ) ;
#3076 = CARTESIAN_POINT ( 'NONE',  ( 13.40780655258104836, 26.42202358648260940, 5.467569244659290284 ) ) ;
#3077 = DIRECTION ( 'NONE',  ( -0.000000000000000000, -0.000000000000000000, -1.000000000000000000 ) ) ;
#3078 = CARTESIAN_POINT ( 'NONE',  ( -174.7835321302054865, 68.75545066608756883, 1.999999999999994893 ) ) ;
#3079 = CIRCLE ( 'NONE', #4303, 25.00000000000000000 ) ;
#3080 = LINE ( 'NONE', #5008, #4607 ) ;
#3081 = ORIENTED_EDGE ( 'NONE', *, *, #753, .F. ) ;
#3082 = AXIS2_PLACEMENT_3D ( 'NONE', #3230, #702, #2648 ) ;
#3083 = AXIS2_PLACEMENT_3D ( 'NONE', #1704, #5131, #238 ) ;
#3084 = DIRECTION ( 'NONE',  ( 0.000000000000000000, 0.000000000000000000, 1.000000000000000000 ) ) ;
#3085 = CARTESIAN_POINT ( 'NONE',  ( 237.0000000000000284, 68.99999999999997158, 0.000000000000000000 ) ) ;
#3086 = ORIENTED_EDGE ( 'NONE', *, *, #499, .T. ) ;
#3087 = DIRECTION ( 'NONE',  ( -0.000000000000000000, 0.000000000000000000, 1.000000000000000000 ) ) ;
#3088 = VERTEX_POINT ( 'NONE', #3947 ) ;
#3089 = VECTOR ( 'NONE', #3407, 1000.000000000000000 ) ;
#3090 = CARTESIAN_POINT ( 'NONE',  ( 42.00000000000000000, 69.00000000000000000, 110.0000000000000000 ) ) ;
#3091 = DIRECTION ( 'NONE',  ( -0.000000000000000000, -0.000000000000000000, 1.000000000000000000 ) ) ;
#3092 = CARTESIAN_POINT ( 'NONE',  ( 0.000000000000000000, 0.000000000000000000, 48.00000000000000000 ) ) ;
#3093 = EDGE_LOOP ( 'NONE', ( #3032, #5488 ) ) ;
#3094 = DIRECTION ( 'NONE',  ( -1.000000000000000000, 1.224646799147352961E-16, 0.000000000000000000 ) ) ;
#3095 = CARTESIAN_POINT ( 'NONE',  ( 0.000000000000000000, 0.000000000000000000, 12.00000000000000000 ) ) ;
#3096 = CARTESIAN_POINT ( 'NONE',  ( 6.710385028064199453, 21.99961506306615178, 35.13225475196805547 ) ) ;
#3097 = CARTESIAN_POINT ( 'NONE',  ( 5.896395598744648581, 24.30897383879703710, 9.016004279442030978 ) ) ;
#3098 = DIRECTION ( 'NONE',  ( 0.000000000000000000, 0.000000000000000000, -1.000000000000000000 ) ) ;
#3099 = EDGE_LOOP ( 'NONE', ( #4132, #5874 ) ) ;
#3100 = ORIENTED_EDGE ( 'NONE', *, *, #3334, .T. ) ;
#3101 = EDGE_LOOP ( 'NONE', ( #1868, #1152, #163, #2526 ) ) ;
#3102 = DIRECTION ( 'NONE',  ( -0.000000000000000000, 0.000000000000000000, -1.000000000000000000 ) ) ;
#3103 = DIRECTION ( 'NONE',  ( -1.000000000000000000, 0.000000000000000000, 0.000000000000000000 ) ) ;
#3104 = DIRECTION ( 'NONE',  ( -1.000000000000000000, 0.000000000000000000, 0.000000000000000000 ) ) ;
#3105 = CARTESIAN_POINT ( 'NONE',  ( -0.2052511266214760433, -21.25619793154163517, -95.00000000000000000 ) ) ;
#3106 = DIRECTION ( 'NONE',  ( -0.000000000000000000, -0.000000000000000000, -1.000000000000000000 ) ) ;
#3107 = ORIENTED_EDGE ( 'NONE', *, *, #3611, .F. ) ;
#3108 = DIRECTION ( 'NONE',  ( 1.000000000000000000, 0.000000000000000000, 0.000000000000000000 ) ) ;
#3109 = APPLICATION_PROTOCOL_DEFINITION ( 'draft international standard', 'automotive_design', 1998, #2379 ) ;
#3110 = DIRECTION ( 'NONE',  ( 1.000000000000000000, 0.000000000000000000, 0.000000000000000000 ) ) ;
#3111 = VECTOR ( 'NONE', #3222, 1000.000000000000000 ) ;
#3112 = ORIENTED_EDGE ( 'NONE', *, *, #2998, .T. ) ;
#3113 = DIRECTION ( 'NONE',  ( 0.000000000000000000, 0.000000000000000000, -1.000000000000000000 ) ) ;
#3114 = ORIENTED_EDGE ( 'NONE', *, *, #947, .T. ) ;
#3115 = CARTESIAN_POINT ( 'NONE',  ( -17.00000000000000355, -25.00000000000000000, -160.0000000000000000 ) ) ;
#3116 = DIRECTION ( 'NONE',  ( 0.000000000000000000, 0.000000000000000000, -1.000000000000000000 ) ) ;
#3117 = DIRECTION ( 'NONE',  ( 0.000000000000000000, 1.000000000000000000, 0.000000000000000000 ) ) ;
#3118 = CARTESIAN_POINT ( 'NONE',  ( 22.21770253897382474, 3.871672004622519037, -160.0000000000000284 ) ) ;
#3119 = ORIENTED_EDGE ( 'NONE', *, *, #1539, .T. ) ;
#3120 = DIRECTION ( 'NONE',  ( -0.000000000000000000, -0.000000000000000000, -1.000000000000000000 ) ) ;
#3121 = PRODUCT_DEFINITION_SHAPE ( 'NONE', 'NONE',  #6368 ) ;
#3122 = CARTESIAN_POINT ( 'NONE',  ( 0.000000000000000000, -4.890878601256026467E-15, 281.0000000000000000 ) ) ;
#3123 = CARTESIAN_POINT ( 'NONE',  ( -1.568280873051609348, 22.94756140746006778, 24.43729500028611312 ) ) ;
#3124 = CARTESIAN_POINT ( 'NONE',  ( -6.736323264042104242, 24.07882193050101449, 8.680799421305115615 ) ) ;
#3125 = DIRECTION ( 'NONE',  ( -0.000000000000000000, -0.000000000000000000, 1.000000000000000000 ) ) ;
#3126 = EDGE_LOOP ( 'NONE', ( #3924, #1318, #4052, #5422 ) ) ;
#3127 = EDGE_CURVE ( 'NONE', #3088, #5213, #4625, .T. ) ;
#3128 = EDGE_LOOP ( 'NONE', ( #1797, #268, #4045, #224 ) ) ;
#3129 = EDGE_CURVE ( 'NONE', #5596, #2909, #1496, .T. ) ;
#3130 = DIRECTION ( 'NONE',  ( -1.000000000000000000, 0.000000000000000000, 0.000000000000000000 ) ) ;
#3131 = EDGE_CURVE ( 'NONE', #1557, #3426, #2766, .T. ) ;
#3132 = DIRECTION ( 'NONE',  ( 0.000000000000000000, -0.000000000000000000, -1.000000000000000000 ) ) ;
#3133 = DIRECTION ( 'NONE',  ( 0.000000000000000000, 0.000000000000000000, 1.000000000000000000 ) ) ;
#3134 = DIRECTION ( 'NONE',  ( 0.000000000000000000, 0.000000000000000000, -1.000000000000000000 ) ) ;
#3135 = LINE ( 'NONE', #5112, #89 ) ;
#3136 = ORIENTED_EDGE ( 'NONE', *, *, #4360, .F. ) ;
#3137 = VECTOR ( 'NONE', #6346, 1000.000000000000000 ) ;
#3138 = CIRCLE ( 'NONE', #377, 20.00000000000000000 ) ;
#3139 = DIRECTION ( 'NONE',  ( 0.000000000000000000, 0.000000000000000000, 1.000000000000000000 ) ) ;
#3140 = LINE ( 'NONE', #710, #6239 ) ;
#3141 = ORIENTED_EDGE ( 'NONE', *, *, #6249, .T. ) ;
#3142 = FACE_OUTER_BOUND ( 'NONE', #3835, .T. ) ;
#3143 = ORIENTED_EDGE ( 'NONE', *, *, #2349, .T. ) ;
#3144 = ADVANCED_FACE ( 'NONE', ( #4673 ), #1650, .F. ) ;
#3145 = VECTOR ( 'NONE', #4354, 1000.000000000000000 ) ;
#3146 = AXIS2_PLACEMENT_3D ( 'NONE', #2691, #4659, #289 ) ;
#3147 =( LENGTH_UNIT ( ) NAMED_UNIT ( * ) SI_UNIT ( .MILLI., .METRE. ) );
#3148 = DIRECTION ( 'NONE',  ( 0.000000000000000000, 0.000000000000000000, -1.000000000000000000 ) ) ;
#3149 = DIRECTION ( 'NONE',  ( -0.000000000000000000, -1.000000000000000000, -0.000000000000000000 ) ) ;
#3150 = CARTESIAN_POINT ( 'NONE',  ( 7.947562104483774093, 68.75545066608756883, 12.00000000000000000 ) ) ;
#3151 = CARTESIAN_POINT ( 'NONE',  ( 1.353091841878393042, -19.95700839110197933, 39.15972426387312311 ) ) ;
#3152 = VERTEX_POINT ( 'NONE', #2098 ) ;
#3153 = VECTOR ( 'NONE', #6340, 1000.000000000000000 ) ;
#3154 =( LENGTH_UNIT ( ) NAMED_UNIT ( * ) SI_UNIT ( .MILLI., .METRE. ) );
#3155 = CARTESIAN_POINT ( 'NONE',  ( 6.979603745006294879, 21.91560538710199779, 29.02082494059217765 ) ) ;
#3156 =( REPRESENTATION_RELATIONSHIP ('NONE','NONE', #632, #3711 ) REPRESENTATION_RELATIONSHIP_WITH_TRANSFORMATION ( #5861 )SHAPE_REPRESENTATION_RELATIONSHIP( ) );
#3157 = CIRCLE ( 'NONE', #6259, 1.000000000000000000 ) ;
#3158 = CARTESIAN_POINT ( 'NONE',  ( 11.89524262375574892, 21.99145298458226705, 5.444687415670879993 ) ) ;
#3159 = DIRECTION ( 'NONE',  ( -0.000000000000000000, -0.000000000000000000, -1.000000000000000000 ) ) ;
#3160 = EDGE_LOOP ( 'NONE', ( #5273, #2735, #4458, #421, #3990, #6313, #2044, #1498 ) ) ;
#3161 = ORIENTED_EDGE ( 'NONE', *, *, #4098, .F. ) ;
#3162 = AXIS2_PLACEMENT_3D ( 'NONE', #749, #4111, #4503 ) ;
#3163 = DIRECTION ( 'NONE',  ( -0.000000000000000000, -0.000000000000000000, -1.000000000000000000 ) ) ;
#3164 = DIRECTION ( 'NONE',  ( -0.000000000000000000, -0.000000000000000000, -1.000000000000000000 ) ) ;
#3165 = CARTESIAN_POINT ( 'NONE',  ( -3.061616997868383043E-15, -25.00000000000000000, -95.00000000000000000 ) ) ;
#3166 = VECTOR ( 'NONE', #4650, 1000.000000000000000 ) ;
#3167 = LINE ( 'NONE', #3621, #5002 ) ;
#3168 = LINE ( 'NONE', #737, #3166 ) ;
#3169 = ORIENTED_EDGE ( 'NONE', *, *, #5355, .F. ) ;
#3170 = CIRCLE ( 'NONE', #4926, 166.8359700257217071 ) ;
#3171 = FILL_AREA_STYLE_COLOUR ( '', #4198 ) ;
#3172 = CARTESIAN_POINT ( 'NONE',  ( -12.25547752887834818, -19.46581264560981239, 5.111654144181065895 ) ) ;
#3173 = AXIS2_PLACEMENT_3D ( 'NONE', #3847, #5241, #828 ) ;
#3174 = ORIENTED_EDGE ( 'NONE', *, *, #2464, .F. ) ;
#3175 = CIRCLE ( 'NONE', #6166, 67.50000000000000000 ) ;
#3176 = PRODUCT_DEFINITION_SHAPE ( 'NONE', 'NONE',  #6363 ) ;
#3177 = DIRECTION ( 'NONE',  ( -1.000000000000000000, 0.000000000000000000, 0.000000000000000000 ) ) ;
#3178 = EDGE_LOOP ( 'NONE', ( #5769, #1016 ) ) ;
#3179 = CIRCLE ( 'NONE', #4517, 19.00000000000000000 ) ;
#3180 = CARTESIAN_POINT ( 'NONE',  ( 0.000000000000000000, 0.000000000000000000, 5.000000000000004441 ) ) ;
#3181 = LINE ( 'NONE', #3770, #2074 ) ;
#3182 = DIRECTION ( 'NONE',  ( 1.000000000000000000, 0.000000000000000000, 0.000000000000000000 ) ) ;
#3183 = CIRCLE ( 'NONE', #1752, 25.00000000000000000 ) ;
#3184 = DIRECTION ( 'NONE',  ( -0.000000000000000000, 0.000000000000000000, 1.000000000000000000 ) ) ;
#3185 = ORIENTED_EDGE ( 'NONE', *, *, #6023, .T. ) ;
#3186 = DIRECTION ( 'NONE',  ( 1.000000000000000000, 0.000000000000000000, 0.000000000000000000 ) ) ;
#3187 = DIRECTION ( 'NONE',  ( -0.000000000000000000, -0.000000000000000000, -1.000000000000000000 ) ) ;
#3188 = CARTESIAN_POINT ( 'NONE',  ( 5.121424986093042087, 22.42477833501277829, 37.27216187635247024 ) ) ;
#3189 = CARTESIAN_POINT ( 'NONE',  ( 13.14183123006952947, -39.58265509608667543, -65.00000000000000000 ) ) ;
#3190 = CLOSED_SHELL ( 'NONE', ( #2257, #4177, #6006, #3203, #600, #5358, #4414, #1907, #2505, #1599, #4676, #1403, #2812, #4405, #1161, #4083, #2625, #2951, #3735, #3728, #1410, #2597, #2180, #4146, #1714, #3414, #2315, #401, #4110, #6311, #6148, #983, #3459, #4590, #3211, #1168, #3874, #5500, #5303, #773, #1137, #5497, #5031, #2738, #4194, #670, #2968, #4063, #4866, #2270, #603, #746, #1806, #6171, #3502, #785, #387, #1926, #3545, #2103, #2309, #6180, #2267, #2404, #2778, #271, #3643, #5229, #1729, #1173, #3058, #5737, #2942, #1155 ) ) ;
#3191 = AXIS2_PLACEMENT_3D ( 'NONE', #4519, #5924, #608 ) ;
#3192 = CARTESIAN_POINT ( 'NONE',  ( 7.199721615955812837, -21.84420850452976026, 33.88807004839755166 ) ) ;
#3193 = ORIENTED_EDGE ( 'NONE', *, *, #2303, .F. ) ;
#3194 = ORIENTED_EDGE ( 'NONE', *, *, #3425, .F. ) ;
#3195 = CARTESIAN_POINT ( 'NONE',  ( -19.25293315802950644, 8.385974291186926166, 12.00000000000000000 ) ) ;
#3196 = DIRECTION ( 'NONE',  ( 0.000000000000000000, 0.000000000000000000, -1.000000000000000000 ) ) ;
#3197 = CARTESIAN_POINT ( 'NONE',  ( -44.43364355155666345, 29.42304313293565343, -65.00000000000000000 ) ) ;
#3198 = DIRECTION ( 'NONE',  ( 1.000000000000000000, 0.000000000000000000, 0.000000000000000000 ) ) ;
#3199 = AXIS2_PLACEMENT_3D ( 'NONE', #564, #3116, #2935 ) ;
#3200 = ORIENTED_EDGE ( 'NONE', *, *, #2936, .T. ) ;
#3201 = CARTESIAN_POINT ( 'NONE',  ( 16.23652742703164620, 37.28747423195200383, 15.00000000000000000 ) ) ;
#3202 = ORIENTED_EDGE ( 'NONE', *, *, #3690, .T. ) ;
#3203 = ADVANCED_FACE ( 'NONE', ( #5197 ), #694, .T. ) ;
#3204 = CARTESIAN_POINT ( 'NONE',  ( 59.99991398172927859, 30.92345909152286154, 276.0000000000000000 ) ) ;
#3205 = CARTESIAN_POINT ( 'NONE',  ( -12.82303992477784860, -19.09670753041942959, 4.547733370409773990 ) ) ;
#3206 = EDGE_LOOP ( 'NONE', ( #6100, #574, #4437, #2919 ) ) ;
#3207 = FACE_OUTER_BOUND ( 'NONE', #4543, .T. ) ;
#3208 = VERTEX_POINT ( 'NONE', #6037 ) ;
#3209 = EDGE_CURVE ( 'NONE', #1679, #394, #3592, .T. ) ;
#3210 = AXIS2_PLACEMENT_3D ( 'NONE', #2971, #6354, #5947 ) ;
#3211 = ADVANCED_FACE ( 'NONE', ( #2641 ), #4148, .T. ) ;
#3212 = UNCERTAINTY_MEASURE_WITH_UNIT (LENGTH_MEASURE( 1.000000000000000082E-05 ), #486, 'distance_accuracy_value', 'NONE');
#3213 = DIRECTION ( 'NONE',  ( -1.000000000000000000, 0.000000000000000000, 0.000000000000000000 ) ) ;
#3214 = FACE_OUTER_BOUND ( 'NONE', #3206, .T. ) ;
#3215 = FACE_OUTER_BOUND ( 'NONE', #3072, .T. ) ;
#3216 = CARTESIAN_POINT ( 'NONE',  ( -4.580917930799676796, -24.58016474715296340, 37.73350732204198721 ) ) ;
#3217 = ORIENTED_EDGE ( 'NONE', *, *, #5426, .T. ) ;
#3218 = EDGE_CURVE ( 'NONE', #1244, #2595, #1615, .T. ) ;
#3219 = CARTESIAN_POINT ( 'NONE',  ( -12.24406280880444164, 19.48300239097275721, 5.141666792244760309 ) ) ;
#3220 = VERTEX_POINT ( 'NONE', #3578 ) ;
#3221 = CARTESIAN_POINT ( 'NONE',  ( 7.438449848406675002, 23.86776331625856784, 32.76532521224501693 ) ) ;
#3222 = DIRECTION ( 'NONE',  ( 0.000000000000000000, 0.000000000000000000, -1.000000000000000000 ) ) ;
#3223 = DIRECTION ( 'NONE',  ( 1.000000000000000000, 0.000000000000000000, -0.000000000000000000 ) ) ;
#3224 = LINE ( 'NONE', #1129, #5253 ) ;
#3225 = VERTEX_POINT ( 'NONE', #2676 ) ;
#3226 = EDGE_LOOP ( 'NONE', ( #1051, #4545, #2690, #1039 ) ) ;
#3227 = CYLINDRICAL_SURFACE ( 'NONE', #4548, 14.00000000000001243 ) ;
#3228 = CARTESIAN_POINT ( 'NONE',  ( 13.85467998626346997, -20.81921389911401832, 3.398299129130501139 ) ) ;
#3229 = PRODUCT ( 'Part 32,6_Varsay\X2\0131\X0\lan', 'Part 32,6_Varsay\X2\0131\X0\lan', '', ( #5445 ) ) ;
#3230 = CARTESIAN_POINT ( 'NONE',  ( 0.000000000000000000, 0.000000000000000000, 23.00000000000000000 ) ) ;
#3231 = DIRECTION ( 'NONE',  ( 1.000000000000000000, 0.000000000000000000, 0.000000000000000000 ) ) ;
#3232 = ORIENTED_EDGE ( 'NONE', *, *, #2075, .F. ) ;
#3233 = DIRECTION ( 'NONE',  ( -0.000000000000000000, -0.000000000000000000, -1.000000000000000000 ) ) ;
#3234 = VERTEX_POINT ( 'NONE', #4610 ) ;
#3235 = CARTESIAN_POINT ( 'NONE',  ( 0.000000000000000000, 0.000000000000000000, -160.0000000000000284 ) ) ;
#3236 = CARTESIAN_POINT ( 'NONE',  ( 3.443445423526525051, -22.74486015987870147, 9.669004251864722121 ) ) ;
#3237 = EDGE_LOOP ( 'NONE', ( #1969, #5048, #937, #2407 ) ) ;
#3238 = EDGE_CURVE ( 'NONE', #5661, #4613, #2733, .T. ) ;
#3239 = LINE ( 'NONE', #4300, #115 ) ;
#3240 = ORIENTED_EDGE ( 'NONE', *, *, #2867, .T. ) ;
#3241 = AXIS2_PLACEMENT_3D ( 'NONE', #1546, #3987, #4531 ) ;
#3242 =( REPRESENTATION_RELATIONSHIP ('NONE','NONE', #632, #5606 ) REPRESENTATION_RELATIONSHIP_WITH_TRANSFORMATION ( #4099 )SHAPE_REPRESENTATION_RELATIONSHIP( ) );
#3243 = CIRCLE ( 'NONE', #1078, 14.00000000000001243 ) ;
#3244 = CARTESIAN_POINT ( 'NONE',  ( 0.2052511266213280505, 21.25619793154159964, -240.0000000000000000 ) ) ;
#3245 = EDGE_CURVE ( 'NONE', #3758, #5734, #3224, .T. ) ;
#3246 = LINE ( 'NONE', #2992, #1248 ) ;
#3247 = CYLINDRICAL_SURFACE ( 'NONE', #5855, 17.00000000000000000 ) ;
#3248 = CARTESIAN_POINT ( 'NONE',  ( -1.953660101606557564, -24.92823101129173580, 24.51724137628377420 ) ) ;
#3249 = ORIENTED_EDGE ( 'NONE', *, *, #2483, .F. ) ;
#3250 = CIRCLE ( 'NONE', #5941, 6.500000000000000000 ) ;
#3251 = SURFACE_STYLE_USAGE ( .BOTH. , #814 ) ;
#3252 = EDGE_LOOP ( 'NONE', ( #601, #3107, #4287, #4928 ) ) ;
#3253 = CARTESIAN_POINT ( 'NONE',  ( 7.401918722292613495, 23.87915698552384924, 33.00856600121883133 ) ) ;
#3254 = DIRECTION ( 'NONE',  ( 0.000000000000000000, -1.000000000000000000, -1.740526192617802767E-17 ) ) ;
#3255 = ADVANCED_FACE ( 'NONE', ( #2702 ), #4085, .F. ) ;
#3256 = VECTOR ( 'NONE', #1912, 1000.000000000000000 ) ;
#3257 = EDGE_CURVE ( 'NONE', #3828, #1896, #1111, .T. ) ;
#3258 = CARTESIAN_POINT ( 'NONE',  ( 0.000000000000000000, 0.000000000000000000, -248.0000000000000000 ) ) ;
#3259 = CARTESIAN_POINT ( 'NONE',  ( 4.579678590235491065, -24.58038806634821682, 37.73441246790280701 ) ) ;
#3260 = VERTEX_POINT ( 'NONE', #3383 ) ;
#3261 = ORIENTED_EDGE ( 'NONE', *, *, #1253, .T. ) ;
#3262 = EDGE_CURVE ( 'NONE', #1020, #4754, #6355, .T. ) ;
#3263 = CARTESIAN_POINT ( 'NONE',  ( -7.306265819825862096, 23.90859775135293219, 30.06340984243353276 ) ) ;
#3264 = AXIS2_PLACEMENT_3D ( 'NONE', #1835, #3831, #5289 ) ;
#3265 = DIRECTION ( 'NONE',  ( -1.000000000000000000, 0.000000000000000000, -0.000000000000000000 ) ) ;
#3266 = CARTESIAN_POINT ( 'NONE',  ( 64.99991398172927859, 32.11307465182860454, 281.0000000000000000 ) ) ;
#3267 = DIRECTION ( 'NONE',  ( 0.000000000000000000, 0.000000000000000000, 1.000000000000000000 ) ) ;
#3268 = AXIS2_PLACEMENT_3D ( 'NONE', #2838, #4714, #3297 ) ;
#3269 = ORIENTED_EDGE ( 'NONE', *, *, #5908, .F. ) ;
#3270 = ORIENTED_EDGE ( 'NONE', *, *, #2931, .F. ) ;
#3271 = EDGE_CURVE ( 'NONE', #3765, #5357, #4419, .T. ) ;
#3272 = CIRCLE ( 'NONE', #510, 89.87058297576894006 ) ;
#3273 = CARTESIAN_POINT ( 'NONE',  ( -0.4786673552078670735, -22.99919074915722916, 9.998953803578743305 ) ) ;
#3274 = CARTESIAN_POINT ( 'NONE',  ( 25.00000000000000000, 3.061616997868383043E-15, 55.00000000000000711 ) ) ;
#3275 = ORIENTED_EDGE ( 'NONE', *, *, #5155, .F. ) ;
#3276 = DIRECTION ( 'NONE',  ( -0.000000000000000000, -0.000000000000000000, -1.000000000000000000 ) ) ;
#3277 = EDGE_LOOP ( 'NONE', ( #5062, #1348, #6184, #1977 ) ) ;
#3278 = COLOUR_RGB ( '',0.7921568627450980005, 0.8196078431372548767, 0.9333333333333333481 ) ;
#3279 = B_SPLINE_CURVE_WITH_KNOTS ( 'NONE', 3,
 ( #1974, #3512, #4378, #2447, #5364, #975, #4417, #10, #495, #456, #5393, #5419, #3937, #4966, #5910, #1458, #2965, #558 ),
 .UNSPECIFIED., .F., .F.,
 ( 4, 2, 2, 2, 2, 2, 2, 2, 4 ),
 ( 0.006348828280262476358, 0.007141278029982640538, 0.007933727779702805585, 0.008726177529422968898, 0.009518627279143133946, 0.01031107702886330073, 0.01110352677858346578, 0.01189597652830363256, 0.01268842627802379761 ),
 .UNSPECIFIED. ) ;
#3280 = DIRECTION ( 'NONE',  ( -0.000000000000000000, -0.000000000000000000, -1.000000000000000000 ) ) ;
#3281 = DIRECTION ( 'NONE',  ( 1.000000000000000000, 0.000000000000000000, 0.000000000000000000 ) ) ;
#3282 = CARTESIAN_POINT ( 'NONE',  ( 279.0000000000000000, 68.99999999999997158, 0.000000000000000000 ) ) ;
#3283 = ORIENTED_EDGE ( 'NONE', *, *, #5236, .F. ) ;
#3284 = CARTESIAN_POINT ( 'NONE',  ( -44.00000000000000000, -13.41640786499873172, -240.0000000000000000 ) ) ;
#3286 = EDGE_LOOP ( 'NONE', ( #4443, #4903, #5433, #593, #1943, #2317 ) ) ;
#3285 = VECTOR ( 'NONE', #1299, 1000.000000000000000 ) ;
#3287 = FACE_OUTER_BOUND ( 'NONE', #1505, .T. ) ;
#3288 = CARTESIAN_POINT ( 'NONE',  ( 0.000000000000000000, 0.000000000000000000, 55.00000000000000711 ) ) ;
#3289 = AXIS2_PLACEMENT_3D ( 'NONE', #986, #4910, #6007 ) ;
#3290 = CARTESIAN_POINT ( 'NONE',  ( 0.000000000000000000, 0.000000000000000000, 47.00000000000000711 ) ) ;
#3291 = CARTESIAN_POINT ( 'NONE',  ( 3.329879077396678877, -24.78142485916624693, 38.51307783140496355 ) ) ;
#3292 = ORIENTED_EDGE ( 'NONE', *, *, #1241, .T. ) ;
#3293 = EDGE_LOOP ( 'NONE', ( #2600, #1860, #6053, #1162 ) ) ;
#3294 = CIRCLE ( 'NONE', #4430, 4.000000000000003553 ) ;
#3295 = CARTESIAN_POINT ( 'NONE',  ( -4.574218739510392595, 24.57872545437487233, 25.82634213602822726 ) ) ;
#3296 = CARTESIAN_POINT ( 'NONE',  ( 0.000000000000000000, 0.000000000000000000, 39.00000000000001421 ) ) ;
#3297 = DIRECTION ( 'NONE',  ( 1.000000000000000000, 0.000000000000000000, 0.000000000000000000 ) ) ;
#3298 = CARTESIAN_POINT ( 'NONE',  ( 17.05141243254543681, -12.25762350764760455, 12.00000000000000000 ) ) ;
#3299 = EDGE_LOOP ( 'NONE', ( #1451, #2661, #3677, #71 ) ) ;
#3300 = ORIENTED_EDGE ( 'NONE', *, *, #482, .F. ) ;
#3301 = VECTOR ( 'NONE', #5710, 1000.000000000000000 ) ;
#3302 = ORIENTED_EDGE ( 'NONE', *, *, #4879, .F. ) ;
#3303 = DIRECTION ( 'NONE',  ( -0.000000000000000000, -0.000000000000000000, -1.000000000000000000 ) ) ;
#3304 = CARTESIAN_POINT ( 'NONE',  ( 17.00000000000000000, 25.00000000000000355, -195.0000000000000000 ) ) ;
#3305 = ORIENTED_EDGE ( 'NONE', *, *, #588, .T. ) ;
#3306 = DIRECTION ( 'NONE',  ( 0.000000000000000000, -1.000000000000000000, 0.000000000000000000 ) ) ;
#3307 = VERTEX_POINT ( 'NONE', #1487 ) ;
#3308 = CARTESIAN_POINT ( 'NONE',  ( 174.7835321302054865, 68.75545066608756883, 0.000000000000000000 ) ) ;
#3309 = LINE ( 'NONE', #4305, #22 ) ;
#3310 = CYLINDRICAL_SURFACE ( 'NONE', #294, 25.00000000000000000 ) ;
#3311 = CARTESIAN_POINT ( 'NONE',  ( -7.246617758453442804, -23.92680898849839721, 29.82624669321133482 ) ) ;
#3312 = ORIENTED_EDGE ( 'NONE', *, *, #1584, .T. ) ;
#3313 =( NAMED_UNIT ( * ) PLANE_ANGLE_UNIT ( ) SI_UNIT ( $, .RADIAN. ) );
#3314 = CARTESIAN_POINT ( 'NONE',  ( 6.097143767825691008, 24.24550159253068671, 36.14924867743860659 ) ) ;
#3315 = DIRECTION ( 'NONE',  ( -0.000000000000000000, -0.000000000000000000, 1.000000000000000000 ) ) ;
#3316 = FACE_OUTER_BOUND ( 'NONE', #1380, .T. ) ;
#3317 = CARTESIAN_POINT ( 'NONE',  ( 4.375754180095211332, -24.61494036324241108, 25.67889403490024236 ) ) ;
#3318 = ORIENTED_EDGE ( 'NONE', *, *, #5945, .F. ) ;
#3319 = EDGE_LOOP ( 'NONE', ( #3461, #904, #3495, #13 ) ) ;
#3320 = CARTESIAN_POINT ( 'NONE',  ( -4.579678590235483959, 24.58038806634820972, 37.73441246790279990 ) ) ;
#3321 = DIRECTION ( 'NONE',  ( -1.000000000000000000, 0.000000000000000000, 0.000000000000000000 ) ) ;
#3322 = FACE_OUTER_BOUND ( 'NONE', #6331, .T. ) ;
#3323 = CARTESIAN_POINT ( 'NONE',  ( -8.000000000000007105, 72.93807001241029297, 1.999999999999974021 ) ) ;
#3324 = EDGE_CURVE ( 'NONE', #5434, #5103, #1958, .T. ) ;
#3325 = ORIENTED_EDGE ( 'NONE', *, *, #3898, .T. ) ;
#3326 = ORIENTED_EDGE ( 'NONE', *, *, #299, .T. ) ;
#3327 = ORIENTED_EDGE ( 'NONE', *, *, #2577, .F. ) ;
#3328 = DIRECTION ( 'NONE',  ( -1.734723475976809855E-15, -1.000000000000000000, 0.000000000000000000 ) ) ;
#3329 = CARTESIAN_POINT ( 'NONE',  ( -13.19716647944431642, 27.23303957064661418, 8.463596398456378012 ) ) ;
#3330 = ADVANCED_FACE ( 'NONE', ( #2897 ), #4475, .T. ) ;
#3331 = EDGE_CURVE ( 'NONE', #6017, #1209, #284, .T. ) ;
#3332 = DIRECTION ( 'NONE',  ( 0.000000000000000000, 0.000000000000000000, -1.000000000000000000 ) ) ;
#3333 = VERTEX_POINT ( 'NONE', #2063 ) ;
#3334 = EDGE_CURVE ( 'NONE', #2995, #602, #4100, .T. ) ;
#3335 = CYLINDRICAL_SURFACE ( 'NONE', #4166, 19.00000000000000000 ) ;
#3336 = PRODUCT_DEFINITION ( 'UNKNOWN', '', #3025, #5707 ) ;
#3337 = DIRECTION ( 'NONE',  ( 0.000000000000000000, -0.000000000000000000, 1.000000000000000000 ) ) ;
#3338 = EDGE_CURVE ( 'NONE', #5491, #1339, #1747, .T. ) ;
#3339 = CARTESIAN_POINT ( 'NONE',  ( -44.00000000000000000, -13.41640786499873172, 0.000000000000000000 ) ) ;
#3340 = CARTESIAN_POINT ( 'NONE',  ( 0.2052511266213299934, 21.25619793154162807, -180.0000000000000000 ) ) ;
#3341 = ORIENTED_EDGE ( 'NONE', *, *, #1626, .T. ) ;
#3342 = ADVANCED_FACE ( 'NONE', ( #5421 ), #5508, .T. ) ;
#3343 = EDGE_CURVE ( 'NONE', #3894, #4348, #5971, .T. ) ;
#3344 = LINE ( 'NONE', #1004, #3137 ) ;
#3345 = CIRCLE ( 'NONE', #2016, 16.00000000000000355 ) ;
#3346 = LINE ( 'NONE', #1814, #2744 ) ;
#3347 = CARTESIAN_POINT ( 'NONE',  ( 2.425736827820245356, -24.88619925908220409, 38.88876102270705104 ) ) ;
#3348 = ORIENTED_EDGE ( 'NONE', *, *, #2734, .T. ) ;
#3349 = DIRECTION ( 'NONE',  ( -1.000000000000000000, -0.000000000000000000, -0.000000000000000000 ) ) ;
#3350 = ORIENTED_EDGE ( 'NONE', *, *, #2547, .T. ) ;
#3351 = DIRECTION ( 'NONE',  ( 1.000000000000000000, 0.000000000000000000, -0.000000000000000000 ) ) ;
#3352 = LINE ( 'NONE', #2873, #3256 ) ;
#3353 = CIRCLE ( 'NONE', #86, 12.50000000000001421 ) ;
#3354 = DIRECTION ( 'NONE',  ( 0.000000000000000000, 0.000000000000000000, 1.000000000000000000 ) ) ;
#3355 = CARTESIAN_POINT ( 'NONE',  ( 0.000000000000000000, 0.000000000000000000, 110.0000000000000000 ) ) ;
#3356 = ORIENTED_EDGE ( 'NONE', *, *, #4671, .T. ) ;
#3357 = VERTEX_POINT ( 'NONE', #2514 ) ;
#3358 = AXIS2_PLACEMENT_3D ( 'NONE', #3663, #1250, #5120 ) ;
#3359 = ORIENTED_EDGE ( 'NONE', *, *, #2982, .F. ) ;
#3360 = DIRECTION ( 'NONE',  ( 0.000000000000000000, 1.000000000000000000, 1.247733429937938623E-16 ) ) ;
#3361 = APPLICATION_CONTEXT ( 'automotive_design' ) ;
#3362 = CONTEXT_DEPENDENT_SHAPE_REPRESENTATION ( #6218, #4617 ) ;
#3363 = PLANE ( 'NONE',  #3379 ) ;
#3364 = VECTOR ( 'NONE', #4997, 1000.000000000000000 ) ;
#3365 = B_SPLINE_CURVE_WITH_KNOTS ( 'NONE', 3,
 ( #491, #1453, #4412, #1511 ),
 .UNSPECIFIED., .F., .F.,
 ( 4, 4 ),
 ( 0.000000000000000000, 0.002032958594636732723 ),
 .UNSPECIFIED. ) ;
#3366 = FACE_OUTER_BOUND ( 'NONE', #5366, .T. ) ;
#3367 = VERTEX_POINT ( 'NONE', #5879 ) ;
#3368 = MECHANICAL_DESIGN_GEOMETRIC_PRESENTATION_REPRESENTATION (  '', ( #1210 ), #3065 ) ;
#3369 = CONTEXT_DEPENDENT_SHAPE_REPRESENTATION ( #1932, #1165 ) ;
#3370 = AXIS2_PLACEMENT_3D ( 'NONE', #1572, #3091, #4077 ) ;
#3371 = CARTESIAN_POINT ( 'NONE',  ( 0.000000000000000000, 0.000000000000000000, 39.00000000000001421 ) ) ;
#3372 = CARTESIAN_POINT ( 'NONE',  ( 0.000000000000000000, 0.000000000000000000, 0.000000000000000000 ) ) ;
#3373 = CARTESIAN_POINT ( 'NONE',  ( -7.502604696612909407, -21.74191879359210944, 31.88172732429694989 ) ) ;
#3374 = CARTESIAN_POINT ( 'NONE',  ( 44.64065620456912598, 28.99954194078667413, -110.0000000000000000 ) ) ;
#3375 = AXIS2_PLACEMENT_3D ( 'NONE', #3410, #5, #2479 ) ;
#3376 = CARTESIAN_POINT ( 'NONE',  ( 44.00000000000009948, 13.41640786499835514, -110.0000000000000000 ) ) ;
#3377 = ORIENTED_EDGE ( 'NONE', *, *, #2653, .F. ) ;
#3378 = DIRECTION ( 'NONE',  ( 1.000000000000000000, 0.000000000000000000, 0.000000000000000000 ) ) ;
#3379 = AXIS2_PLACEMENT_3D ( 'NONE', #2882, #4853, #1921 ) ;
#3380 = DIRECTION ( 'NONE',  ( -0.000000000000000000, -0.000000000000000000, -1.000000000000000000 ) ) ;
#3381 = DIRECTION ( 'NONE',  ( 0.000000000000000000, 0.000000000000000000, 1.000000000000000000 ) ) ;
#3382 = AXIS2_PLACEMENT_3D ( 'NONE', #3757, #468, #5722 ) ;
#3383 = CARTESIAN_POINT ( 'NONE',  ( 13.14183123006952947, -39.58265509608667543, -160.0000000000000284 ) ) ;
#3384 = ORIENTED_EDGE ( 'NONE', *, *, #1892, .F. ) ;
#3385 = CIRCLE ( 'NONE', #4199, 89.87058297576892585 ) ;
#3386 = CARTESIAN_POINT ( 'NONE',  ( -44.43364355155666345, 29.42304313293564988, -110.0000000000000000 ) ) ;
#3387 = CARTESIAN_POINT ( 'NONE',  ( 147.0000000000000284, 69.00000000000000000, 110.0000000000000000 ) ) ;
#3388 = CARTESIAN_POINT ( 'NONE',  ( 7.443729366988918004E-21, -23.00000000000000000, 24.27501000028010125 ) ) ;
#3389 = CIRCLE ( 'NONE', #727, 46.00000000000000000 ) ;
#3390 = DIRECTION ( 'NONE',  ( 0.000000000000000000, 0.000000000000000000, 1.000000000000000000 ) ) ;
#3391 = DIRECTION ( 'NONE',  ( 1.000000000000000000, -1.734723475976809855E-15, 0.000000000000000000 ) ) ;
#3392 = DIRECTION ( 'NONE',  ( -1.000000000000000000, 0.000000000000000000, 0.000000000000000000 ) ) ;
#3393 = EDGE_CURVE ( 'NONE', #6099, #3894, #3389, .T. ) ;
#3394 = EDGE_LOOP ( 'NONE', ( #4764, #379, #6206, #348 ) ) ;
#3395 = EDGE_LOOP ( 'NONE', ( #106, #695, #2819, #3939, #3030, #386, #5694, #2791 ) ) ;
#3396 = VERTEX_POINT ( 'NONE', #3417 ) ;
#3397 = DIRECTION ( 'NONE',  ( 0.000000000000000000, -0.000000000000000000, 1.000000000000000000 ) ) ;
#3398 = CARTESIAN_POINT ( 'NONE',  ( 0.000000000000000000, 0.000000000000000000, 301.0000000000000568 ) ) ;
#3399 = AXIS2_PLACEMENT_3D ( 'NONE', #688, #5098, #5127 ) ;
#3400 = CIRCLE ( 'NONE', #5054, 21.00000000000000355 ) ;
#3401 = CARTESIAN_POINT ( 'NONE',  ( -3.415902643629519009, -24.76920443774479352, 9.674315651764088031 ) ) ;
#3402 = ORIENTED_EDGE ( 'NONE', *, *, #5427, .F. ) ;
#3403 = ADVANCED_FACE ( 'NONE', ( #5454 ), #3002, .T. ) ;
#3404 = DIRECTION ( 'NONE',  ( 1.852483853906148040E-16, -1.000000000000000000, -1.239088197126290570E-16 ) ) ;
#3405 = CARTESIAN_POINT ( 'NONE',  ( -7.368286983821151992, -21.78790057683621129, 30.30389194166913569 ) ) ;
#3406 = DIRECTION ( 'NONE',  ( -0.000000000000000000, 0.000000000000000000, 1.000000000000000000 ) ) ;
#3407 = DIRECTION ( 'NONE',  ( -0.000000000000000000, -0.000000000000000000, 1.000000000000000000 ) ) ;
#3408 = VERTEX_POINT ( 'NONE', #4504 ) ;
#3409 = EDGE_CURVE ( 'NONE', #661, #2368, #5557, .T. ) ;
#3410 = CARTESIAN_POINT ( 'NONE',  ( -44.64065620456893413, -28.99954194078699032, -195.0000000000000000 ) ) ;
#3411 = EDGE_CURVE ( 'NONE', #4956, #4783, #42, .T. ) ;
#3412 = FACE_OUTER_BOUND ( 'NONE', #4576, .T. ) ;
#3413 = EDGE_CURVE ( 'NONE', #590, #1163, #2002, .T. ) ;
#3414 = ADVANCED_FACE ( 'NONE', ( #5999, #1573 ), #5942, .T. ) ;
#3415 = EDGE_CURVE ( 'NONE', #2696, #4920, #5911, .T. ) ;
#3416 = FACE_OUTER_BOUND ( 'NONE', #2832, .T. ) ;
#3417 = CARTESIAN_POINT ( 'NONE',  ( -25.00000000000000000, 0.000000000000000000, 47.00000000000000711 ) ) ;
#3418 = EDGE_LOOP ( 'NONE', ( #5921, #2704, #2717, #2642 ) ) ;
#3419 = ORIENTED_EDGE ( 'NONE', *, *, #313, .T. ) ;
#3420 = CARTESIAN_POINT ( 'NONE',  ( -3.667391228670915382, 22.70656428659075843, 38.32101890234235242 ) ) ;
#3421 = CARTESIAN_POINT ( 'NONE',  ( 19.00000000000000000, 2.326828918379970970E-15, 23.00000000000000000 ) ) ;
#3422 = DIRECTION ( 'NONE',  ( -0.000000000000000000, 0.000000000000000000, -1.000000000000000000 ) ) ;
#3423 = CYLINDRICAL_SURFACE ( 'NONE', #4934, 89.87058297576894006 ) ;
#3424 = ORIENTED_EDGE ( 'NONE', *, *, #5906, .T. ) ;
#3425 = EDGE_CURVE ( 'NONE', #6099, #1071, #458, .T. ) ;
#3426 = VERTEX_POINT ( 'NONE', #3633 ) ;
#3427 = ORIENTED_EDGE ( 'NONE', *, *, #2795, .T. ) ;
#3428 = ORIENTED_EDGE ( 'NONE', *, *, #2763, .T. ) ;
#3429 = CARTESIAN_POINT ( 'NONE',  ( 0.000000000000000000, 0.000000000000000000, 50.00000000000000711 ) ) ;
#3430 = DIRECTION ( 'NONE',  ( -0.000000000000000000, -0.000000000000000000, 1.000000000000000000 ) ) ;
#3431 = FACE_BOUND ( 'NONE', #2326, .T. ) ;
#3432 = ORIENTED_EDGE ( 'NONE', *, *, #4883, .F. ) ;
#3433 = FACE_OUTER_BOUND ( 'NONE', #3537, .T. ) ;
#3434 = CARTESIAN_POINT ( 'NONE',  ( 132.0000000000000000, 69.00000000000000000, 0.000000000000000000 ) ) ;
#3435 = DIRECTION ( 'NONE',  ( 0.000000000000000000, 0.000000000000000000, 1.000000000000000000 ) ) ;
#3436 = DIRECTION ( 'NONE',  ( -0.000000000000000000, -0.000000000000000000, -1.000000000000000000 ) ) ;
#3437 = ADVANCED_FACE ( 'NONE', ( #2182 ), #5577, .F. ) ;
#3438 = CARTESIAN_POINT ( 'NONE',  ( -174.7835321302054865, 68.75545066608756883, 12.00000000000000000 ) ) ;
#3439 = CARTESIAN_POINT ( 'NONE',  ( 0.2052511266213280505, 21.25619793154159964, 15.00000000000000000 ) ) ;
#3440 = VERTEX_POINT ( 'NONE', #5095 ) ;
#3441 = DIRECTION ( 'NONE',  ( -0.000000000000000000, -0.000000000000000000, -1.000000000000000000 ) ) ;
#3442 = CARTESIAN_POINT ( 'NONE',  ( 0.000000000000000000, 0.000000000000000000, -4.000000000000000000 ) ) ;
#3443 = ADVANCED_FACE ( 'NONE', ( #4663 ), #5025, .F. ) ;
#3444 = EDGE_CURVE ( 'NONE', #1742, #4844, #5641, .T. ) ;
#3445 = CARTESIAN_POINT ( 'NONE',  ( 13.14183123006952947, -39.58265509608667543, -160.0000000000000284 ) ) ;
#3446 = DIRECTION ( 'NONE',  ( 1.000000000000000000, 0.000000000000000000, 0.000000000000000000 ) ) ;
#3447 = ORIENTED_EDGE ( 'NONE', *, *, #946, .F. ) ;
#3448 = CARTESIAN_POINT ( 'NONE',  ( 73.99999999999987210, 76.99999716619419132, 5.000000000000000000 ) ) ;
#3449 = EDGE_CURVE ( 'NONE', #5709, #2780, #4209, .T. ) ;
#3450 = CARTESIAN_POINT ( 'NONE',  ( 172.0000000000000000, 68.99999999999998579, 110.0000000000000000 ) ) ;
#3451 = AXIS2_PLACEMENT_3D ( 'NONE', #493, #4802, #2857 ) ;
#3452 = FACE_OUTER_BOUND ( 'NONE', #4373, .T. ) ;
#3453 = EDGE_CURVE ( 'NONE', #116, #3948, #38, .T. ) ;
#3454 = VECTOR ( 'NONE', #770, 1000.000000000000000 ) ;
#3455 = DIRECTION ( 'NONE',  ( 0.000000000000000000, 0.000000000000000000, -1.000000000000000000 ) ) ;
#3456 = DIRECTION ( 'NONE',  ( -1.000000000000000000, 0.000000000000000000, 0.000000000000000000 ) ) ;
#3457 = LINE ( 'NONE', #2519, #2981 ) ;
#3458 = ORIENTED_EDGE ( 'NONE', *, *, #5527, .T. ) ;
#3459 = ADVANCED_FACE ( 'NONE', ( #2606 ), #1183, .T. ) ;
#3460 = VERTEX_POINT ( 'NONE', #5124 ) ;
#3461 = ORIENTED_EDGE ( 'NONE', *, *, #4671, .F. ) ;
#3462 = CIRCLE ( 'NONE', #1603, 19.00000000000000000 ) ;
#3463 = CIRCLE ( 'NONE', #691, 17.00000000000000000 ) ;
#3464 = ORIENTED_EDGE ( 'NONE', *, *, #3943, .T. ) ;
#3465 = CARTESIAN_POINT ( 'NONE',  ( 12.72367524380681658, 29.12081030169099805, 2.199628915743095714 ) ) ;
#3466 = CARTESIAN_POINT ( 'NONE',  ( -43.99999999999987921, 13.41640786499904969, -110.0000000000000000 ) ) ;
#3467 = EDGE_CURVE ( 'NONE', #453, #3504, #3179, .T. ) ;
#3468 = AXIS2_PLACEMENT_3D ( 'NONE', #4857, #4923, #2409 ) ;
#3469 = DIRECTION ( 'NONE',  ( 0.000000000000000000, 0.000000000000000000, 1.000000000000000000 ) ) ;
#3470 = ORIENTED_EDGE ( 'NONE', *, *, #1118, .F. ) ;
#3471 = AXIS2_PLACEMENT_3D ( 'NONE', #3873, #5791, #1366 ) ;
#3472 = DIRECTION ( 'NONE',  ( 7.920214157681025148E-17, 1.271205363195804239E-14, 1.000000000000000000 ) ) ;
#3473 = CARTESIAN_POINT ( 'NONE',  ( 25.00000000000000000, 0.000000000000000000, -20.00000000000000000 ) ) ;
#3474 = DIRECTION ( 'NONE',  ( -0.000000000000000000, -0.000000000000000000, -1.000000000000000000 ) ) ;
#3475 = EDGE_LOOP ( 'NONE', ( #1889, #5933, #1024, #2101 ) ) ;
#3476 = ORIENTED_EDGE ( 'NONE', *, *, #130, .T. ) ;
#3477 = DIRECTION ( 'NONE',  ( 1.000000000000000000, 0.000000000000000000, 0.000000000000000000 ) ) ;
#3478 = AXIS2_PLACEMENT_3D ( 'NONE', #5740, #1312, #5702 ) ;
#3479 = DIRECTION ( 'NONE',  ( -0.000000000000000000, 0.000000000000000000, -1.000000000000000000 ) ) ;
#3480 = CARTESIAN_POINT ( 'NONE',  ( 2.432532833620817403, 24.88553977760507152, 24.66355118963700832 ) ) ;
#3481 = AXIS2_PLACEMENT_3D ( 'NONE', #1624, #2525, #3590 ) ;
#3482 = LINE ( 'NONE', #1904, #72 ) ;
#3483 = DIRECTION ( 'NONE',  ( -1.852483853906148040E-16, 1.000000000000000000, 0.000000000000000000 ) ) ;
#3484 = ORIENTED_EDGE ( 'NONE', *, *, #3245, .T. ) ;
#3485 = CARTESIAN_POINT ( 'NONE',  ( 15.99408614349810698, 16.52843635781563592, 0.000000000000000000 ) ) ;
#3486 = VECTOR ( 'NONE', #3031, 1000.000000000000000 ) ;
#3487 = CARTESIAN_POINT ( 'NONE',  ( 13.40794989232620615, 26.42147665086397623, 6.529465147186706453 ) ) ;
#3488 = FACE_BOUND ( 'NONE', #1375, .T. ) ;
#3489 = PLANE ( 'NONE',  #3001 ) ;
#3490 = CIRCLE ( 'NONE', #1112, 22.67164836619066648 ) ;
#3491 = DIRECTION ( 'NONE',  ( 0.000000000000000000, -0.000000000000000000, -1.000000000000000000 ) ) ;
#3492 = AXIS2_PLACEMENT_3D ( 'NONE', #2017, #1502, #3978 ) ;
#3493 = DIRECTION ( 'NONE',  ( -0.000000000000000000, -0.000000000000000000, -1.000000000000000000 ) ) ;
#3494 = ORIENTED_EDGE ( 'NONE', *, *, #753, .T. ) ;
#3495 = ORIENTED_EDGE ( 'NONE', *, *, #4286, .T. ) ;
#3496 = AXIS2_PLACEMENT_3D ( 'NONE', #3521, #5036, #1093 ) ;
#3497 = ADVANCED_FACE ( 'NONE', ( #170 ), #3666, .F. ) ;
#3498 = CARTESIAN_POINT ( 'NONE',  ( 12.41746183822997551, 30.39531364385071299, 1.999999999999990008 ) ) ;
#3499 = CARTESIAN_POINT ( 'NONE',  ( 0.000000000000000000, 0.000000000000000000, 0.000000000000000000 ) ) ;
#3500 = AXIS2_PLACEMENT_3D ( 'NONE', #2121, #4078, #4601 ) ;
#3501 = ADVANCED_FACE ( 'NONE', ( #1217 ), #2213, .T. ) ;
#3502 = ADVANCED_FACE ( 'NONE', ( #4534, #2092 ), #6091, .F. ) ;
#3503 = CARTESIAN_POINT ( 'NONE',  ( 0.000000000000000000, 0.000000000000000000, 23.00000000000000000 ) ) ;
#3504 = VERTEX_POINT ( 'NONE', #4044 ) ;
#3505 = AXIS2_PLACEMENT_3D ( 'NONE', #5190, #779, #4699 ) ;
#3506 = APPLICATION_PROTOCOL_DEFINITION ( 'draft international standard', 'automotive_design', 1998, #4893 ) ;
#3507 = CARTESIAN_POINT ( 'NONE',  ( -6.381573266039188397, -22.09732860014628031, 35.72159715675526570 ) ) ;
#3508 = DIRECTION ( 'NONE',  ( 1.000000000000000000, 0.000000000000000000, 0.000000000000000000 ) ) ;
#3509 = EDGE_LOOP ( 'NONE', ( #2108, #6332, #1265, #2300, #2478, #1634, #6173 ) ) ;
#3510 = DIRECTION ( 'NONE',  ( 0.000000000000000000, 0.000000000000000000, 1.000000000000000000 ) ) ;
#3511 = CARTESIAN_POINT ( 'NONE',  ( -25.00000000000000000, 0.000000000000000000, 55.00000000000000711 ) ) ;
#3512 = CARTESIAN_POINT ( 'NONE',  ( -13.41482486054669465, 26.39531364385071655, 5.735664331006448791 ) ) ;
#3513 = AXIS2_PLACEMENT_3D ( 'NONE', #5290, #4732, #6187 ) ;
#3514 = DIRECTION ( 'NONE',  ( -0.000000000000000000, -0.000000000000000000, -1.000000000000000000 ) ) ;
#3515 = EDGE_LOOP ( 'NONE', ( #3885, #3359 ) ) ;
#3516 = DIRECTION ( 'NONE',  ( 1.000000000000000000, 0.000000000000000000, 0.000000000000000000 ) ) ;
#3517 = CARTESIAN_POINT ( 'NONE',  ( 44.64065620456912598, 28.99954194078667413, -175.0000000000000284 ) ) ;
#3518 = CARTESIAN_POINT ( 'NONE',  ( 4.240673024049072204, 22.60901396202200075, 25.57291330172528987 ) ) ;
#3519 = FACE_OUTER_BOUND ( 'NONE', #1795, .T. ) ;
#3520 = ADVANCED_FACE ( 'NONE', ( #2695 ), #138, .F. ) ;
#3521 = CARTESIAN_POINT ( 'NONE',  ( -0.2052511266214760433, -21.25619793154163517, -115.0000000000000000 ) ) ;
#3522 = VERTEX_POINT ( 'NONE', #1151 ) ;
#3523 = ORIENTED_EDGE ( 'NONE', *, *, #595, .F. ) ;
#3524 = ORIENTED_EDGE ( 'NONE', *, *, #5147, .T. ) ;
#3525 = ADVANCED_FACE ( 'NONE', ( #2634 ), #3571, .F. ) ;
#3526 = CARTESIAN_POINT ( 'NONE',  ( 15.99408614349810698, -16.52843635781563592, 0.000000000000000000 ) ) ;
#3527 = EDGE_CURVE ( 'NONE', #2013, #823, #3700, .T. ) ;
#3528 = CARTESIAN_POINT ( 'NONE',  ( 44.00000000000000000, -13.41640786499874771, -225.0000000000000000 ) ) ;
#3529 = PLANE ( 'NONE',  #1221 ) ;
#3530 = CARTESIAN_POINT ( 'NONE',  ( -13.84152781008413946, -20.82799749684992108, 3.414623522204553563 ) ) ;
#3531 = ORIENTED_EDGE ( 'NONE', *, *, #5749, .T. ) ;
#3532 = EDGE_CURVE ( 'NONE', #2050, #1163, #1353, .T. ) ;
#3533 = EDGE_CURVE ( 'NONE', #4515, #3234, #1646, .T. ) ;
#3534 = APPLICATION_PROTOCOL_DEFINITION ( 'draft international standard', 'automotive_design', 1998, #2911 ) ;
#3535 = CARTESIAN_POINT ( 'NONE',  ( -17.00000000000000000, 0.000000000000000000, -180.0000000000000000 ) ) ;
#3536 = CYLINDRICAL_SURFACE ( 'NONE', #834, 20.00000000000000000 ) ;
#3537 = EDGE_LOOP ( 'NONE', ( #6041, #1708, #2043, #4880 ) ) ;
#3538 = EDGE_CURVE ( 'NONE', #4754, #1020, #575, .T. ) ;
#3539 = ADVANCED_FACE ( 'NONE', ( #2439 ), #4552, .F. ) ;
#3540 = CARTESIAN_POINT ( 'NONE',  ( 6.500000000000000000, 0.000000000000000000, 48.00000000000000000 ) ) ;
#3541 = EDGE_CURVE ( 'NONE', #2388, #221, #1254, .T. ) ;
#3542 = LINE ( 'NONE', #5639, #802 ) ;
#3543 = CARTESIAN_POINT ( 'NONE',  ( -22.21770253897380343, -3.871672004622680241, -30.00000000000000000 ) ) ;
#3544 = EDGE_LOOP ( 'NONE', ( #5599, #3998, #3841, #4578 ) ) ;
#3545 = ADVANCED_FACE ( 'NONE', ( #6253 ), #4339, .T. ) ;
#3546 = CYLINDRICAL_SURFACE ( 'NONE', #1730, 17.00000000000000000 ) ;
#3547 = DIRECTION ( 'NONE',  ( -2.295390878742131754E-32, 1.239088197126290570E-16, -1.000000000000000000 ) ) ;
#3548 = CARTESIAN_POINT ( 'NONE',  ( 7.502466904913718260, 21.74196656924153714, 31.65671859158186763 ) ) ;
#3549 = CARTESIAN_POINT ( 'NONE',  ( 59.99991398172927859, 30.92345909152286154, 5.000000000000004441 ) ) ;
#3550 = DIRECTION ( 'NONE',  ( -0.000000000000000000, -0.000000000000000000, -1.000000000000000000 ) ) ;
#3551 = VERTEX_POINT ( 'NONE', #426 ) ;
#3552 = ORIENTED_EDGE ( 'NONE', *, *, #5288, .F. ) ;
#3553 = AXIS2_PLACEMENT_3D ( 'NONE', #5586, #3163, #5074 ) ;
#3554 = VERTEX_POINT ( 'NONE', #6318 ) ;
#3555 = DIRECTION ( 'NONE',  ( -0.000000000000000000, -0.000000000000000000, -1.000000000000000000 ) ) ;
#3556 = CARTESIAN_POINT ( 'NONE',  ( 13.41482486054666268, 26.39531364385071299, 5.735664331006449679 ) ) ;
#3557 = DIRECTION ( 'NONE',  ( 0.000000000000000000, 0.000000000000000000, -1.000000000000000000 ) ) ;
#3558 = LINE ( 'NONE', #5899, #1613 ) ;
#3559 = CARTESIAN_POINT ( 'NONE',  ( 0.000000000000000000, 0.000000000000000000, 48.00000000000000000 ) ) ;
#3560 = ORIENTED_EDGE ( 'NONE', *, *, #2499, .F. ) ;
#3561 = AXIS2_PLACEMENT_3D ( 'NONE', #6168, #3132, #826 ) ;
#3562 = APPLICATION_PROTOCOL_DEFINITION ( 'draft international standard', 'automotive_design', 1998, #5226 ) ;
#3563 = CARTESIAN_POINT ( 'NONE',  ( -174.7835321302054865, 68.75545066608756883, 0.000000000000000000 ) ) ;
#3564 = VECTOR ( 'NONE', #1252, 1000.000000000000000 ) ;
#3565 = ORIENTED_EDGE ( 'NONE', *, *, #3943, .F. ) ;
#3566 = CARTESIAN_POINT ( 'NONE',  ( 0.000000000000000000, 0.000000000000000000, 0.000000000000000000 ) ) ;
#3567 = ORIENTED_EDGE ( 'NONE', *, *, #1722, .F. ) ;
#3568 = DIRECTION ( 'NONE',  ( -0.000000000000000000, -0.000000000000000000, -1.000000000000000000 ) ) ;
#3569 = CARTESIAN_POINT ( 'NONE',  ( 44.00000000000000000, -13.41640786499873705, -180.0000000000000000 ) ) ;
#3570 = AXIS2_PLACEMENT_3D ( 'NONE', #5751, #2829, #1324 ) ;
#3571 = PLANE ( 'NONE',  #1225 ) ;
#3572 = ORIENTED_EDGE ( 'NONE', *, *, #322, .T. ) ;
#3573 = CARTESIAN_POINT ( 'NONE',  ( -11.01859089670589675, 20.20136408472527023, 6.200517937480644726 ) ) ;
#3574 = CARTESIAN_POINT ( 'NONE',  ( 132.0000000000000000, 69.00000000000000000, 110.0000000000000000 ) ) ;
#3575 = CARTESIAN_POINT ( 'NONE',  ( -5.578949544899560742, 22.31500106593816213, 26.74243945601464745 ) ) ;
#3576 = VECTOR ( 'NONE', #6325, 1000.000000000000000 ) ;
#3577 = CARTESIAN_POINT ( 'NONE',  ( 3.415902643629519009, 24.76920443774479352, 9.674315651764088031 ) ) ;
#3578 = CARTESIAN_POINT ( 'NONE',  ( 44.00000000000000000, -13.41640786499873705, -195.0000000000000000 ) ) ;
#3579 = ORIENTED_EDGE ( 'NONE', *, *, #2473, .F. ) ;
#3580 = AXIS2_PLACEMENT_3D ( 'NONE', #5744, #2825, #6192 ) ;
#3581 = ORIENTED_EDGE ( 'NONE', *, *, #5830, .F. ) ;
#3582 = ORIENTED_EDGE ( 'NONE', *, *, #482, .T. ) ;
#3583 = ORIENTED_EDGE ( 'NONE', *, *, #3271, .T. ) ;
#3584 = DIRECTION ( 'NONE',  ( 0.000000000000000000, 0.000000000000000000, 1.000000000000000000 ) ) ;
#3585 = AXIS2_PLACEMENT_3D ( 'NONE', #5965, #3510, #1057 ) ;
#3586 = CARTESIAN_POINT ( 'NONE',  ( 12.84176997259613273, 28.64101934588368081, 2.395886979664402894 ) ) ;
#3587 = CARTESIAN_POINT ( 'NONE',  ( 13.14183123006966980, -39.58265509608656174, -115.0000000000000000 ) ) ;
#3588 = CARTESIAN_POINT ( 'NONE',  ( 0.000000000000000000, 0.000000000000000000, 50.00000000000000711 ) ) ;
#3589 = AXIS2_PLACEMENT_3D ( 'NONE', #4716, #3134, #3198 ) ;
#3590 = DIRECTION ( 'NONE',  ( 0.000000000000000000, -1.000000000000000000, 0.000000000000000000 ) ) ;
#3591 = ORIENTED_EDGE ( 'NONE', *, *, #5930, .T. ) ;
#3592 = CIRCLE ( 'NONE', #4425, 23.00000000000000000 ) ;
#3593 = DIRECTION ( 'NONE',  ( -3.030207807088497008E-18, -3.568357447238533958E-17, 1.000000000000000000 ) ) ;
#3594 = DIRECTION ( 'NONE',  ( 1.000000000000000000, 0.000000000000000000, 0.000000000000000000 ) ) ;
#3595 = ORIENTED_EDGE ( 'NONE', *, *, #2294, .T. ) ;
#3596 = LINE ( 'NONE', #4561, #2058 ) ;
#3597 = ORIENTED_EDGE ( 'NONE', *, *, #5263, .T. ) ;
#3598 = AXIS2_PLACEMENT_3D ( 'NONE', #3439, #5413, #4927 ) ;
#3599 = DIRECTION ( 'NONE',  ( 1.000000000000000000, 0.000000000000000000, 0.000000000000000000 ) ) ;
#3600 = FACE_OUTER_BOUND ( 'NONE', #3782, .T. ) ;
#3601 = EDGE_CURVE ( 'NONE', #3061, #2498, #4521, .T. ) ;
#3602 = CARTESIAN_POINT ( 'NONE',  ( 7.500000000000000000, 9.184850993605147944E-16, 48.00000000000000000 ) ) ;
#3603 = ADVANCED_FACE ( 'NONE', ( #4216 ), #1994, .T. ) ;
#3604 = DIRECTION ( 'NONE',  ( -1.000000000000000000, 0.000000000000000000, 0.000000000000000000 ) ) ;
#3605 = ORIENTED_EDGE ( 'NONE', *, *, #4837, .T. ) ;
#3606 = VECTOR ( 'NONE', #756, 1000.000000000000000 ) ;
#3607 = DIRECTION ( 'NONE',  ( 1.000000000000000000, 0.000000000000000000, 0.000000000000000000 ) ) ;
#3608 = EDGE_CURVE ( 'NONE', #1146, #4872, #3183, .T. ) ;
#3609 = CARTESIAN_POINT ( 'NONE',  ( -7.512701611559312376, 21.73844013154226218, 31.66439142681324981 ) ) ;
#3610 = EDGE_CURVE ( 'NONE', #5091, #6324, #3931, .T. ) ;
#3611 = EDGE_CURVE ( 'NONE', #1995, #2333, #62, .T. ) ;
#3612 = AXIS2_PLACEMENT_3D ( 'NONE', #1770, #4661, #254 ) ;
#3613 = DIRECTION ( 'NONE',  ( -1.000000000000000000, -1.852483853906148286E-16, 0.000000000000000000 ) ) ;
#3614 = DIRECTION ( 'NONE',  ( -0.000000000000000000, -0.000000000000000000, 1.000000000000000000 ) ) ;
#3615 = ORIENTED_EDGE ( 'NONE', *, *, #4660, .F. ) ;
#3616 = EDGE_LOOP ( 'NONE', ( #3432, #4028, #5280, #766, #1606, #1072, #3081 ) ) ;
#3617 = DIRECTION ( 'NONE',  ( 1.000000000000000000, 0.000000000000000000, 0.000000000000000000 ) ) ;
#3618 = DIRECTION ( 'NONE',  ( 0.000000000000000000, 1.000000000000000000, 0.000000000000000000 ) ) ;
#3619 = EDGE_CURVE ( 'NONE', #161, #2613, #1001, .T. ) ;
#3620 = DIRECTION ( 'NONE',  ( -1.000000000000000000, -1.852483853906148286E-16, 0.000000000000000000 ) ) ;
#3621 = CARTESIAN_POINT ( 'NONE',  ( -17.05141243254543681, -12.25762350764760455, 12.00000000000000000 ) ) ;
#3622 = CARTESIAN_POINT ( 'NONE',  ( -12.76907600075766247, -21.49559483975649599, 4.603672158788645774 ) ) ;
#3623 = ORIENTED_EDGE ( 'NONE', *, *, #3444, .F. ) ;
#3624 = CARTESIAN_POINT ( 'NONE',  ( 0.000000000000000000, 69.00000000000000000, 0.000000000000000000 ) ) ;
#3625 = CARTESIAN_POINT ( 'NONE',  ( -2.876010458515648960, -22.82309565144259267, 38.71608687161452877 ) ) ;
#3626 = VERTEX_POINT ( 'NONE', #33 ) ;
#3627 = FACE_OUTER_BOUND ( 'NONE', #1218, .T. ) ;
#3628 = VERTEX_POINT ( 'NONE', #5835 ) ;
#3629 = EDGE_CURVE ( 'NONE', #3913, #5889, #2412, .T. ) ;
#3630 =( NAMED_UNIT ( * ) PLANE_ANGLE_UNIT ( ) SI_UNIT ( $, .RADIAN. ) );
#3631 = PLANE ( 'NONE',  #849 ) ;
#3632 = LINE ( 'NONE', #5603, #3678 ) ;
#3633 = CARTESIAN_POINT ( 'NONE',  ( 17.00000000000000000, 0.000000000000000000, -248.0000000000000000 ) ) ;
#3634 = ORIENTED_EDGE ( 'NONE', *, *, #5236, .T. ) ;
#3635 = PRESENTATION_STYLE_ASSIGNMENT (( #1671 ) ) ;
#3636 = PRODUCT_DEFINITION_SHAPE ( 'NONE', 'NONE',  #2864 ) ;
#3637 = LINE ( 'NONE', #398, #4527 ) ;
#3638 = CARTESIAN_POINT ( 'NONE',  ( 5.575863217335945698, 22.31445838370337853, 26.75407420319146823 ) ) ;
#3639 = DIRECTION ( 'NONE',  ( 1.852483853906148040E-16, -1.000000000000000000, 0.000000000000000000 ) ) ;
#3640 = CARTESIAN_POINT ( 'NONE',  ( -10.34785354329971341, 22.76990768458740177, 6.703770685560594522 ) ) ;
#3641 = CARTESIAN_POINT ( 'NONE',  ( 6.716176415091607232, -21.99834172012562661, 35.14285310556104491 ) ) ;
#3642 = ORIENTED_EDGE ( 'NONE', *, *, #4275, .T. ) ;
#3643 = ADVANCED_FACE ( 'NONE', ( #5476 ), #3859, .T. ) ;
#3644 = ORIENTED_EDGE ( 'NONE', *, *, #196, .F. ) ;
#3645 = ORIENTED_EDGE ( 'NONE', *, *, #2082, .T. ) ;
#3646 = LINE ( 'NONE', #606, #1503 ) ;
#3647 = DIRECTION ( 'NONE',  ( 0.000000000000000000, 1.000000000000000000, -0.000000000000000000 ) ) ;
#3648 = CARTESIAN_POINT ( 'NONE',  ( 0.000000000000000000, 0.000000000000000000, 5.000000000000004441 ) ) ;
#3649 = CARTESIAN_POINT ( 'NONE',  ( 7.947562104483774093, 68.75545066608756883, 12.00000000000000000 ) ) ;
#3650 = CARTESIAN_POINT ( 'NONE',  ( 0.000000000000000000, 0.000000000000000000, -175.0000000000000284 ) ) ;
#3651 = VERTEX_POINT ( 'NONE', #1966 ) ;
#3652 = VECTOR ( 'NONE', #2118, 1000.000000000000000 ) ;
#3653 = DIRECTION ( 'NONE',  ( -1.000000000000000000, 0.000000000000000000, 0.000000000000000000 ) ) ;
#3654 = CARTESIAN_POINT ( 'NONE',  ( 4.711348314259845793, -22.51623045471248119, 9.370182291681606657 ) ) ;
#3655 = ORIENTED_EDGE ( 'NONE', *, *, #1449, .T. ) ;
#3656 = CARTESIAN_POINT ( 'NONE',  ( -44.00000000000000000, -13.41640786499873172, 15.00000000000000000 ) ) ;
#3657 = VERTEX_POINT ( 'NONE', #452 ) ;
#3658 = CIRCLE ( 'NONE', #1400, 25.00000000000000000 ) ;
#3659 = MECHANICAL_DESIGN_GEOMETRIC_PRESENTATION_REPRESENTATION (  '', ( #2430 ), #4901 ) ;
#3660 =( NAMED_UNIT ( * ) SI_UNIT ( $, .STERADIAN. ) SOLID_ANGLE_UNIT ( ) );
#3661 = AXIS2_PLACEMENT_3D ( 'NONE', #876, #4662, #256 ) ;
#3662 = UNCERTAINTY_MEASURE_WITH_UNIT (LENGTH_MEASURE( 1.000000000000000082E-05 ), #2204, 'distance_accuracy_value', 'NONE');
#3663 = CARTESIAN_POINT ( 'NONE',  ( 0.000000000000000000, 0.000000000000000000, 0.000000000000000000 ) ) ;
#3664 = DIRECTION ( 'NONE',  ( -1.000000000000000000, -0.000000000000000000, -0.000000000000000000 ) ) ;
#3665 = CARTESIAN_POINT ( 'NONE',  ( 22.00000000000000000, 2.694222958124176809E-15, 44.00000000000000711 ) ) ;
#3666 = CYLINDRICAL_SURFACE ( 'NONE', #3500, 23.00000000000000000 ) ;
#3667 = ORIENTED_EDGE ( 'NONE', *, *, #2265, .T. ) ;
#3668 = AXIS2_PLACEMENT_3D ( 'NONE', #5354, #4860, #902 ) ;
#3669 = CARTESIAN_POINT ( 'NONE',  ( 0.000000000000000000, 0.000000000000000000, 55.00000000000000711 ) ) ;
#3670 =( LENGTH_UNIT ( ) NAMED_UNIT ( * ) SI_UNIT ( .MILLI., .METRE. ) );
#3671 = CARTESIAN_POINT ( 'NONE',  ( 2.012341796004660122, 22.91179784512888773, 39.00000000000001421 ) ) ;
#3672 = CIRCLE ( 'NONE', #4180, 17.00000000000000000 ) ;
#3673 = CARTESIAN_POINT ( 'NONE',  ( 4.673148220383224860, 24.56288069930688067, 9.380541037249376046 ) ) ;
#3674 = CARTESIAN_POINT ( 'NONE',  ( 4.050825139678606135, -22.64130375691644304, 38.09092692957536030 ) ) ;
#3675 = ORIENTED_EDGE ( 'NONE', *, *, #5945, .T. ) ;
#3676 = EDGE_CURVE ( 'NONE', #2535, #6227, #2772, .T. ) ;
#3677 = ORIENTED_EDGE ( 'NONE', *, *, #313, .F. ) ;
#3678 = VECTOR ( 'NONE', #1182, 1000.000000000000000 ) ;
#3679 = CARTESIAN_POINT ( 'NONE',  ( -1.948881123199609711, 24.92505092879368078, 24.52843033598424327 ) ) ;
#3680 = LINE ( 'NONE', #1297, #4693 ) ;
#3681 = DIRECTION ( 'NONE',  ( 1.000000000000000000, 0.000000000000000000, 0.000000000000000000 ) ) ;
#3682 = VECTOR ( 'NONE', #2419, 1000.000000000000000 ) ;
#3683 = FACE_BOUND ( 'NONE', #4449, .T. ) ;
#3684 = EDGE_LOOP ( 'NONE', ( #3727, #2495 ) ) ;
#3685 = ADVANCED_FACE ( 'NONE', ( #5448, #5356 ), #525, .T. ) ;
#3686 = LINE ( 'NONE', #3904, #4710 ) ;
#3687 = ORIENTED_EDGE ( 'NONE', *, *, #1911, .F. ) ;
#3688 = EDGE_CURVE ( 'NONE', #2831, #5896, #3294, .T. ) ;
#3689 = AXIS2_PLACEMENT_3D ( 'NONE', #2725, #5164, #3607 ) ;
#3690 = EDGE_CURVE ( 'NONE', #1488, #5709, #4946, .T. ) ;
#3691 = ADVANCED_FACE ( 'NONE', ( #1029 ), #3959, .F. ) ;
#3692 = DIRECTION ( 'NONE',  ( 1.000000000000000000, 0.000000000000000000, 0.000000000000000000 ) ) ;
#3693 = AXIS2_PLACEMENT_3D ( 'NONE', #6359, #2332, #4482 ) ;
#3694 = ORIENTED_EDGE ( 'NONE', *, *, #5902, .F. ) ;
#3695 = AXIS2_PLACEMENT_3D ( 'NONE', #1534, #3430, #1585 ) ;
#3696 = PRODUCT_DEFINITION_SHAPE ( 'NONE', 'NONE',  #6364 ) ;
#3697 = CARTESIAN_POINT ( 'NONE',  ( 25.00000000000000000, 0.000000000000000000, -20.00000000000000000 ) ) ;
#3698 = ORIENTED_EDGE ( 'NONE', *, *, #2591, .T. ) ;
#3699 = APPLICATION_CONTEXT ( 'automotive_design' ) ;
#3700 = CIRCLE ( 'NONE', #3704, 21.00000000000000355 ) ;
#3701 = CYLINDRICAL_SURFACE ( 'NONE', #4379, 17.00000000000000000 ) ;
#3702 = PLANE ( 'NONE',  #3724 ) ;
#3703 = LINE ( 'NONE', #6252, #3564 ) ;
#3704 = AXIS2_PLACEMENT_3D ( 'NONE', #651, #1804, #4796 ) ;
#3705 = CARTESIAN_POINT ( 'NONE',  ( 1.684770966858813335, -19.93163181623162572, 39.09123673121591480 ) ) ;
#3706 = ORIENTED_EDGE ( 'NONE', *, *, #4270, .T. ) ;
#3707 = FILL_AREA_STYLE ('',( #2636 ) ) ;
#3708 = VERTEX_POINT ( 'NONE', #4372 ) ;
#3709 = CARTESIAN_POINT ( 'NONE',  ( 7.500037790182079611, 23.84846815096122796, 31.28125562555190342 ) ) ;
#3710 = DIRECTION ( 'NONE',  ( 0.000000000000000000, 0.000000000000000000, 1.000000000000000000 ) ) ;
#3711 = SHAPE_REPRESENTATION ( 'Part 32,5_Varsay\X2\0131\X0\lan', ( #6349 ), #596 ) ;
#3712 = VECTOR ( 'NONE', #5733, 1000.000000000000000 ) ;
#3713 = DIRECTION ( 'NONE',  ( 0.000000000000000000, 0.000000000000000000, 1.000000000000000000 ) ) ;
#3714 = VECTOR ( 'NONE', #5511, 1000.000000000000000 ) ;
#3715 = VECTOR ( 'NONE', #3328, 1000.000000000000000 ) ;
#3716 = CARTESIAN_POINT ( 'NONE',  ( 2.012341796004660122, -22.91179784512888773, 39.00000000000001421 ) ) ;
#3717 = ORIENTED_EDGE ( 'NONE', *, *, #5698, .F. ) ;
#3718 = ORIENTED_EDGE ( 'NONE', *, *, #5161, .T. ) ;
#3719 = DIRECTION ( 'NONE',  ( -0.000000000000000000, -0.000000000000000000, -1.000000000000000000 ) ) ;
#3720 = ADVANCED_FACE ( 'NONE', ( #3 ), #1450, .F. ) ;
#3721 = DIRECTION ( 'NONE',  ( 0.000000000000000000, 0.000000000000000000, -1.000000000000000000 ) ) ;
#3722 = LINE ( 'NONE', #4583, #4827 ) ;
#3723 = LINE ( 'NONE', #703, #4510 ) ;
#3724 = AXIS2_PLACEMENT_3D ( 'NONE', #1251, #2243, #3740 ) ;
#3725 = ORIENTED_EDGE ( 'NONE', *, *, #272, .F. ) ;
#3726 = DIRECTION ( 'NONE',  ( 0.000000000000000000, -1.000000000000000000, 0.000000000000000000 ) ) ;
#3727 = ORIENTED_EDGE ( 'NONE', *, *, #1148, .F. ) ;
#3728 = ADVANCED_FACE ( 'NONE', ( #970 ), #2509, .T. ) ;
#3729 = DIRECTION ( 'NONE',  ( 0.000000000000000000, 0.000000000000000000, 1.000000000000000000 ) ) ;
#3730 = CONTEXT_DEPENDENT_SHAPE_REPRESENTATION ( #3906, #3176 ) ;
#3731 = CARTESIAN_POINT ( 'NONE',  ( -6.012884121744077603, -22.20400618356517697, 8.958536348443306707 ) ) ;
#3732 = ORIENTED_EDGE ( 'NONE', *, *, #130, .F. ) ;
#3733 = CARTESIAN_POINT ( 'NONE',  ( 16.99999999999999645, -25.00000000000000000, -95.00000000000000000 ) ) ;
#3734 = EDGE_LOOP ( 'NONE', ( #4755, #1424, #4411, #5471 ) ) ;
#3735 = ADVANCED_FACE ( 'NONE', ( #5900 ), #4985, .T. ) ;
#3736 = EDGE_CURVE ( 'NONE', #3651, #4674, #5598, .T. ) ;
#3737 = LINE ( 'NONE', #5699, #2630 ) ;
#3738 = VECTOR ( 'NONE', #5645, 1000.000000000000000 ) ;
#3739 = DIRECTION ( 'NONE',  ( 1.000000000000000000, 0.000000000000000000, 0.000000000000000000 ) ) ;
#3740 = DIRECTION ( 'NONE',  ( -1.852483853906148040E-16, -1.000000000000000000, 0.000000000000000000 ) ) ;
#3741 = DIRECTION ( 'NONE',  ( 0.000000000000000000, 0.000000000000000000, -1.000000000000000000 ) ) ;
#3742 = ADVANCED_FACE ( 'NONE', ( #193 ), #4106, .F. ) ;
#3743 = CARTESIAN_POINT ( 'NONE',  ( -5.475713916123538638, -24.39360375241166778, 36.90593746307732204 ) ) ;
#3744 = ORIENTED_EDGE ( 'NONE', *, *, #4153, .F. ) ;
#3745 = VERTEX_POINT ( 'NONE', #5117 ) ;
#3746 = CARTESIAN_POINT ( 'NONE',  ( 9.185524248261779151E-16, 25.00000000000000000, 39.27501000028010480 ) ) ;
#3747 = LINE ( 'NONE', #5711, #1501 ) ;
#3748 = EDGE_CURVE ( 'NONE', #43, #1691, #3813, .T. ) ;
#3749 = CARTESIAN_POINT ( 'NONE',  ( -6.500000000000005329, 120.0000000000000000, -4.000000000000000000 ) ) ;
#3750 = CARTESIAN_POINT ( 'NONE',  ( 5.648970382492173314, -24.35596037157666771, 26.81763994746972912 ) ) ;
#3751 = ORIENTED_EDGE ( 'NONE', *, *, #249, .T. ) ;
#3752 = EDGE_LOOP ( 'NONE', ( #3821, #2005, #911, #4150 ) ) ;
#3753 = CARTESIAN_POINT ( 'NONE',  ( -2.425736827820241803, 24.88619925908220054, 38.88876102270705815 ) ) ;
#3754 = PRODUCT_DEFINITION_FORMATION_WITH_SPECIFIED_SOURCE ( 'ANY', '', #4667, .NOT_KNOWN. ) ;
#3755 = DIRECTION ( 'NONE',  ( -1.000000000000000000, -0.000000000000000000, -0.000000000000000000 ) ) ;
#3756 = DIRECTION ( 'NONE',  ( 1.000000000000000000, 0.000000000000000000, 0.000000000000000000 ) ) ;
#3757 = CARTESIAN_POINT ( 'NONE',  ( 0.000000000000000000, 120.0000000000000000, -4.000000000000000000 ) ) ;
#3758 = VERTEX_POINT ( 'NONE', #1692 ) ;
#3759 = ORIENTED_EDGE ( 'NONE', *, *, #5614, .T. ) ;
#3760 = LINE ( 'NONE', #5726, #2575 ) ;
#3761 = CARTESIAN_POINT ( 'NONE',  ( -10.40746208496127245, -20.52425257667962555, 6.660905398399123101 ) ) ;
#3762 = CARTESIAN_POINT ( 'NONE',  ( -13.14183123006980480, 39.58265509608657595, -180.0000000000000000 ) ) ;
#3763 = ORIENTED_EDGE ( 'NONE', *, *, #1246, .F. ) ;
#3764 = CARTESIAN_POINT ( 'NONE',  ( 2.012341796004660122, -19.89850447888114005, 39.00000000000001421 ) ) ;
#3765 = VERTEX_POINT ( 'NONE', #5995 ) ;
#3766 = AXIS2_PLACEMENT_3D ( 'NONE', #301, #2252, #4221 ) ;
#3767 = B_SPLINE_CURVE_WITH_KNOTS ( 'NONE', 3,
 ( #4188, #270, #824, #3783, #3679, #5201, #1295, #307, #4228, #792, #3295, #5235, #1782, #4677, #2705, #5757, #1329, #2809, #5274, #4778, #3263, #5174, #372, #2737, #762, #2293, #2327, #4288, #2225, #6265, #1853, #408, #2773, #4747, #5788, #1364, #3320, #2260, #5300, #3753, #886, #1709, #5652, #343, #5718, #1231 ),
 .UNSPECIFIED., .F., .F.,
 ( 4, 2, 2, 2, 2, 2, 2, 2, 2, 2, 2, 2, 2, 2, 2, 2, 2, 2, 2, 2, 2, 2, 4 ),
 ( 2.472553540688041407E-19, 0.001474063385043944061, 0.002211095077565916091, 0.002948126770087888121, 0.004422190155131833049, 0.005159221847653804212, 0.005896253540175776242, 0.007370316925219718568, 0.008844380310263660894, 0.009581412002785630322, 0.01031844369530760148, 0.01179250708035154208, 0.01326657046539548267, 0.01474063385043942499, 0.01547766554296140483, 0.01621469723548338293, 0.01695172892800536277, 0.01768876062052734260, 0.01916282400557132309, 0.02063688739061530358, 0.02211095077565928407, 0.02284798246818127432, 0.02358501416070326803 ),
 .UNSPECIFIED. ) ;
#3768 = AXIS2_PLACEMENT_3D ( 'NONE', #5898, #3337, #4858 ) ;
#3769 =( NAMED_UNIT ( * ) PLANE_ANGLE_UNIT ( ) SI_UNIT ( $, .RADIAN. ) );
#3770 = CARTESIAN_POINT ( 'NONE',  ( 0.000000000000000000, 0.000000000000000000, 0.000000000000000000 ) ) ;
#3771 = FACE_OUTER_BOUND ( 'NONE', #5518, .T. ) ;
#3772 = CARTESIAN_POINT ( 'NONE',  ( -3.330617891528921515, -24.78132568362454435, 38.51271458136145753 ) ) ;
#3773 = ORIENTED_EDGE ( 'NONE', *, *, #5618, .T. ) ;
#3774 = CIRCLE ( 'NONE', #1296, 166.8359700257217071 ) ;
#3775 = CARTESIAN_POINT ( 'NONE',  ( 25.00000000000000000, 3.061616997868383043E-15, 55.00000000000000711 ) ) ;
#3776 = ORIENTED_EDGE ( 'NONE', *, *, #2848, .F. ) ;
#3777 = CARTESIAN_POINT ( 'NONE',  ( -1.684770966858812891, 19.93163181623162572, 39.09123673121591480 ) ) ;
#3778 = CARTESIAN_POINT ( 'NONE',  ( 2.450084894395748503, 22.87335089571185875, 38.87807751528530531 ) ) ;
#3779 = FACE_BOUND ( 'NONE', #179, .T. ) ;
#3780 = CARTESIAN_POINT ( 'NONE',  ( 3.769188925537579671, -24.71764851934220175, 38.27740560533010949 ) ) ;
#3781 = ORIENTED_EDGE ( 'NONE', *, *, #2721, .T. ) ;
#3782 = EDGE_LOOP ( 'NONE', ( #5191, #4977 ) ) ;
#3783 = CARTESIAN_POINT ( 'NONE',  ( -1.710351842506663500, 24.94259032362968398, 24.46851125284992179 ) ) ;
#3784 = CARTESIAN_POINT ( 'NONE',  ( 0.000000000000000000, 25.00000000000000000, -20.00000000000000000 ) ) ;
#3785 = CYLINDRICAL_SURFACE ( 'NONE', #2639, 90.00000000000319744 ) ;
#3786 = LINE ( 'NONE', #1432, #308 ) ;
#3787 = AXIS2_PLACEMENT_3D ( 'NONE', #4427, #2189, #1128 ) ;
#3788 = VERTEX_POINT ( 'NONE', #5056 ) ;
#3789 = ORIENTED_EDGE ( 'NONE', *, *, #1452, .T. ) ;
#3790 = AXIS2_PLACEMENT_3D ( 'NONE', #480, #1504, #5895 ) ;
#3791 = FACE_OUTER_BOUND ( 'NONE', #3395, .T. ) ;
#3792 = CARTESIAN_POINT ( 'NONE',  ( -8.000000000000021316, 1.481987083124922376E-15, 0.000000000000000000 ) ) ;
#3793 = ORIENTED_EDGE ( 'NONE', *, *, #3045, .F. ) ;
#3794 = DIRECTION ( 'NONE',  ( -0.000000000000000000, -0.000000000000000000, 1.000000000000000000 ) ) ;
#3795 = ORIENTED_EDGE ( 'NONE', *, *, #5837, .F. ) ;
#3796 = CIRCLE ( 'NONE', #1105, 25.00000000000000000 ) ;
#3797 = LINE ( 'NONE', #5287, #2022 ) ;
#3798 = DIRECTION ( 'NONE',  ( -1.000000000000000000, 0.000000000000000000, 0.000000000000000000 ) ) ;
#3799 = DIRECTION ( 'NONE',  ( 0.000000000000000000, 0.000000000000000000, -1.000000000000000000 ) ) ;
#3800 = CARTESIAN_POINT ( 'NONE',  ( -4.376116820636601012, -24.61487579939255710, 25.67915452354946737 ) ) ;
#3801 = ORIENTED_EDGE ( 'NONE', *, *, #5817, .T. ) ;
#3802 = CARTESIAN_POINT ( 'NONE',  ( 0.000000000000000000, 25.00000000000000000, 301.0000000000000568 ) ) ;
#3803 = AXIS2_PLACEMENT_3D ( 'NONE', #79, #1469, #3972 ) ;
#3804 = CARTESIAN_POINT ( 'NONE',  ( 5.641746473127992267, 24.35561814371764910, 36.72278580929200587 ) ) ;
#3805 = DIRECTION ( 'NONE',  ( 1.000000000000000000, 0.000000000000000000, 0.000000000000000000 ) ) ;
#3806 = EDGE_CURVE ( 'NONE', #4674, #258, #1034, .T. ) ;
#3807 = AXIS2_PLACEMENT_3D ( 'NONE', #2153, #1119, #3060 ) ;
#3808 = DIRECTION ( 'NONE',  ( 0.000000000000000000, 0.000000000000000000, 1.000000000000000000 ) ) ;
#3810 = ADVANCED_FACE ( 'NONE', ( #4594 ), #1176, .T. ) ;
#3809 = CARTESIAN_POINT ( 'NONE',  ( 1.957817464472357827, -24.92794428843966514, 39.03180047523677842 ) ) ;
#3811 = ORIENTED_EDGE ( 'NONE', *, *, #3527, .F. ) ;
#3812 = VERTEX_POINT ( 'NONE', #1145 ) ;
#3813 = CIRCLE ( 'NONE', #4836, 17.00000000000000000 ) ;
#3814 = DIRECTION ( 'NONE',  ( 1.000000000000000000, 0.000000000000000000, 0.000000000000000000 ) ) ;
#3815 = AXIS2_PLACEMENT_3D ( 'NONE', #3235, #1688, #2713 ) ;
#3816 = CARTESIAN_POINT ( 'NONE',  ( 17.05141243254541550, -24.25762350764758679, 12.00000000000000000 ) ) ;
#3817 = DIRECTION ( 'NONE',  ( 0.000000000000000000, 0.000000000000000000, 1.000000000000000000 ) ) ;
#3818 = CARTESIAN_POINT ( 'NONE',  ( 0.000000000000000000, 0.000000000000000000, -273.0000000000000000 ) ) ;
#3819 = EDGE_LOOP ( 'NONE', ( #3318, #3725, #771, #1477, #1883, #965, #1229, #4745, #4719, #3021, #2020, #5704 ) ) ;
#3820 = ORIENTED_EDGE ( 'NONE', *, *, #3056, .F. ) ;
#3821 = ORIENTED_EDGE ( 'NONE', *, *, #1922, .T. ) ;
#3822 = PRODUCT_RELATED_PRODUCT_CATEGORY ( 'part', '', ( #657 ) ) ;
#3823 = ADVANCED_FACE ( 'NONE', ( #3142 ), #1633, .F. ) ;
#3824 = DIRECTION ( 'NONE',  ( 0.000000000000000000, 1.000000000000000000, 0.000000000000000000 ) ) ;
#3825 = CARTESIAN_POINT ( 'NONE',  ( -13.00740645622773606, 27.97830129128178811, 9.197704556789860320 ) ) ;
#3826 = VECTOR ( 'NONE', #3149, 1000.000000000000000 ) ;
#3827 = DIRECTION ( 'NONE',  ( 1.000000000000000000, 0.000000000000000000, 0.000000000000000000 ) ) ;
#3828 = VERTEX_POINT ( 'NONE', #1109 ) ;
#3829 = ORIENTED_EDGE ( 'NONE', *, *, #548, .T. ) ;
#3830 = DIRECTION ( 'NONE',  ( 0.000000000000000000, -1.000000000000000000, 0.000000000000000000 ) ) ;
#3831 = DIRECTION ( 'NONE',  ( 1.000000000000000000, -1.317171866856884620E-15, 5.656572562666558182E-16 ) ) ;
#3832 = FACE_BOUND ( 'NONE', #2223, .T. ) ;
#3833 = CARTESIAN_POINT ( 'NONE',  ( -23.00000000000000000, 0.000000000000000000, 0.000000000000000000 ) ) ;
#3834 = CARTESIAN_POINT ( 'NONE',  ( -2.546401178541497462E-16, -25.00000000000000000, 24.27501000028010125 ) ) ;
#3835 = EDGE_LOOP ( 'NONE', ( #279, #4252, #5172, #3193, #2602, #5401 ) ) ;
#3836 = DIRECTION ( 'NONE',  ( -0.000000000000000000, -0.000000000000000000, 1.000000000000000000 ) ) ;
#3837 = CARTESIAN_POINT ( 'NONE',  ( 279.0000000000000000, 0.000000000000000000, 110.0000000000000000 ) ) ;
#3838 = CARTESIAN_POINT ( 'NONE',  ( 3.766262172602996561, 24.71811694763050937, 25.27080528860306430 ) ) ;
#3839 = FACE_OUTER_BOUND ( 'NONE', #3973, .T. ) ;
#3840 = CARTESIAN_POINT ( 'NONE',  ( 5.269070065585171214, -22.39093555978999817, 26.41927588677976502 ) ) ;
#3841 = ORIENTED_EDGE ( 'NONE', *, *, #2000, .T. ) ;
#3842 = CARTESIAN_POINT ( 'NONE',  ( 0.000000000000000000, 0.000000000000000000, 39.00000000000001421 ) ) ;
#3843 = ORIENTED_EDGE ( 'NONE', *, *, #4859, .T. ) ;
#3844 = DIRECTION ( 'NONE',  ( -1.000000000000000000, 0.000000000000000000, 0.000000000000000000 ) ) ;
#3845 = LINE ( 'NONE', #1013, #1046 ) ;
#3846 = CARTESIAN_POINT ( 'NONE',  ( 0.000000000000000000, 0.000000000000000000, 48.00000000000000000 ) ) ;
#3847 = CARTESIAN_POINT ( 'NONE',  ( 174.7835321302054865, 68.75545066608756883, 12.00000000000000000 ) ) ;
#3848 = ORIENTED_EDGE ( 'NONE', *, *, #521, .T. ) ;
#3849 = ORIENTED_EDGE ( 'NONE', *, *, #2265, .F. ) ;
#3850 = ORIENTED_EDGE ( 'NONE', *, *, #2272, .F. ) ;
#3851 = DIRECTION ( 'NONE',  ( 2.295390878742131754E-32, -1.239088197126290570E-16, 1.000000000000000000 ) ) ;
#3852 = CARTESIAN_POINT ( 'NONE',  ( -12.84201764556569536, 28.64001483306500617, 9.603681688880101319 ) ) ;
#3853 = DIRECTION ( 'NONE',  ( 1.000000000000000000, 0.000000000000000000, -0.000000000000000000 ) ) ;
#3854 = ORIENTED_EDGE ( 'NONE', *, *, #5146, .F. ) ;
#3855 = CARTESIAN_POINT ( 'NONE',  ( 0.000000000000000000, 0.000000000000000000, 23.00000000000000000 ) ) ;
#3856 = SHAPE_REPRESENTATION_RELATIONSHIP ( 'NONE' , 'NONE' ,  #1490, #4941 ) ;
#3857 = CARTESIAN_POINT ( 'NONE',  ( -7.502466904913718260, -21.74196656924153714, 31.65671859158186763 ) ) ;
#3858 = DIRECTION ( 'NONE',  ( -0.000000000000000000, -0.000000000000000000, -1.000000000000000000 ) ) ;
#3859 = CYLINDRICAL_SURFACE ( 'NONE', #2989, 89.99999999999998579 ) ;
#3860 = ORIENTED_EDGE ( 'NONE', *, *, #6291, .T. ) ;
#3861 = AXIS2_PLACEMENT_3D ( 'NONE', #5983, #3584, #2615 ) ;
#3862 = CARTESIAN_POINT ( 'NONE',  ( -1.239954884136695111E-14, -67.50000000000000000, 281.0000000000000000 ) ) ;
#3863 = LINE ( 'NONE', #5325, #5412 ) ;
#3864 = CARTESIAN_POINT ( 'NONE',  ( 5.133588784792091353, 24.46788053448572242, 26.30186172257456789 ) ) ;
#3865 = DIRECTION ( 'NONE',  ( -0.000000000000000000, -0.000000000000000000, -1.000000000000000000 ) ) ;
#3866 = CARTESIAN_POINT ( 'NONE',  ( 7.257770128441434210, -23.92352318576051928, 33.72861583961353205 ) ) ;
#3867 = ORIENTED_EDGE ( 'NONE', *, *, #4064, .F. ) ;
#3868 = DIRECTION ( 'NONE',  ( -0.000000000000000000, -0.000000000000000000, -1.000000000000000000 ) ) ;
#3869 = VERTEX_POINT ( 'NONE', #6085 ) ;
#3870 = CARTESIAN_POINT ( 'NONE',  ( -6.505027467542590536, 22.06241888168487009, 35.53465933272089927 ) ) ;
#3871 = DIRECTION ( 'NONE',  ( 0.000000000000000000, -0.000000000000000000, 1.000000000000000000 ) ) ;
#3872 = CIRCLE ( 'NONE', #4814, 6.500000000000005329 ) ;
#3873 = CARTESIAN_POINT ( 'NONE',  ( 0.000000000000000000, 25.00000000000000000, -225.0000000000000000 ) ) ;
#3874 = ADVANCED_FACE ( 'NONE', ( #2146 ), #2088, .T. ) ;
#3875 = DIRECTION ( 'NONE',  ( -0.000000000000000000, -0.000000000000000000, -1.000000000000000000 ) ) ;
#3876 = ORIENTED_EDGE ( 'NONE', *, *, #3994, .F. ) ;
#3877 = ORIENTED_EDGE ( 'NONE', *, *, #1584, .F. ) ;
#3878 = CARTESIAN_POINT ( 'NONE',  ( -17.00000000000000000, 2.081899558550500280E-15, -115.0000000000000000 ) ) ;
#3879 = EDGE_CURVE ( 'NONE', #3788, #2050, #3596, .T. ) ;
#3880 = CARTESIAN_POINT ( 'NONE',  ( -7.500000000000000000, 0.000000000000000000, 48.00000000000000000 ) ) ;
#3881 = CIRCLE ( 'NONE', #1200, 6.500000000000000000 ) ;
#3882 = ADVANCED_FACE ( 'NONE', ( #3627 ), #4039, .F. ) ;
#3883 = CARTESIAN_POINT ( 'NONE',  ( 15.23040061807463630, -19.83277885499231630, 1.438641001509332051 ) ) ;
#3884 = ADVANCED_FACE ( 'NONE', ( #2627 ), #5633, .T. ) ;
#3885 = ORIENTED_EDGE ( 'NONE', *, *, #938, .F. ) ;
#3886 = AXIS2_PLACEMENT_3D ( 'NONE', #6016, #2083, #3043 ) ;
#3887 = AXIS2_PLACEMENT_3D ( 'NONE', #683, #4599, #201 ) ;
#3888 = CYLINDRICAL_SURFACE ( 'NONE', #175, 17.00000000000000000 ) ;
#3889 = EDGE_CURVE ( 'NONE', #1881, #6115, #2115, .T. ) ;
#3890 = ADVANCED_FACE ( 'NONE', ( #6054 ), #3536, .F. ) ;
#3891 = CYLINDRICAL_SURFACE ( 'NONE', #4791, 46.00000000000000000 ) ;
#3892 = DIRECTION ( 'NONE',  ( 1.000000000000000000, -1.852483853906148040E-16, -0.000000000000000000 ) ) ;
#3893 = DIRECTION ( 'NONE',  ( 0.000000000000000000, -1.000000000000000000, 0.000000000000000000 ) ) ;
#3894 = VERTEX_POINT ( 'NONE', #743 ) ;
#3895 = FACE_OUTER_BOUND ( 'NONE', #2274, .T. ) ;
#3896 = DIRECTION ( 'NONE',  ( 1.000000000000000000, 0.000000000000000000, -0.000000000000000000 ) ) ;
#3897 = FACE_BOUND ( 'NONE', #989, .T. ) ;
#3898 = EDGE_CURVE ( 'NONE', #4340, #1760, #2689, .T. ) ;
#3899 = CARTESIAN_POINT ( 'NONE',  ( -44.43364355155666345, 29.42304313293564988, -130.0000000000000000 ) ) ;
#3900 = CIRCLE ( 'NONE', #4724, 25.00000000000000000 ) ;
#3901 = DIRECTION ( 'NONE',  ( 1.000000000000000000, 0.000000000000000000, 0.000000000000000000 ) ) ;
#3902 = ORIENTED_EDGE ( 'NONE', *, *, #4886, .F. ) ;
#3903 = CIRCLE ( 'NONE', #2250, 25.00000000000000000 ) ;
#3904 = CARTESIAN_POINT ( 'NONE',  ( 9.184850993605147944E-16, 25.00000000000000000, 39.27501000028010480 ) ) ;
#3905 = CARTESIAN_POINT ( 'NONE',  ( 16.23652742703164620, 37.28747423195200383, -225.0000000000000000 ) ) ;
#3906 =( REPRESENTATION_RELATIONSHIP ('NONE','NONE', #632, #2313 ) REPRESENTATION_RELATIONSHIP_WITH_TRANSFORMATION ( #4202 )SHAPE_REPRESENTATION_RELATIONSHIP( ) );
#3907 = CYLINDRICAL_SURFACE ( 'NONE', #445, 25.00000000000000000 ) ;
#3908 = FACE_OUTER_BOUND ( 'NONE', #3226, .T. ) ;
#3909 = DIRECTION ( 'NONE',  ( -0.000000000000000000, -0.000000000000000000, 1.000000000000000000 ) ) ;
#3910 = FACE_OUTER_BOUND ( 'NONE', #4788, .T. ) ;
#3911 = ORIENTED_EDGE ( 'NONE', *, *, #1205, .F. ) ;
#3912 = VECTOR ( 'NONE', #333, 1000.000000000000000 ) ;
#3913 = VERTEX_POINT ( 'NONE', #4070 ) ;
#3914 = ORIENTED_EDGE ( 'NONE', *, *, #2763, .F. ) ;
#3915 = ORIENTED_EDGE ( 'NONE', *, *, #2393, .T. ) ;
#3916 = ADVANCED_FACE ( 'NONE', ( #617 ), #4529, .T. ) ;
#3917 = VECTOR ( 'NONE', #2067, 1000.000000000000000 ) ;
#3918 = DIRECTION ( 'NONE',  ( -0.000000000000000000, -0.000000000000000000, -1.000000000000000000 ) ) ;
#3919 = ITEM_DEFINED_TRANSFORMATION ( 'NONE', 'NONE', #4074,  #6349 ) ;
#3920 = CARTESIAN_POINT ( 'NONE',  ( 13.14183123006966980, -39.58265509608656174, -95.00000000000000000 ) ) ;
#3921 = CIRCLE ( 'NONE', #538, 22.00000000000000000 ) ;
#3922 = VECTOR ( 'NONE', #4916, 1000.000000000000000 ) ;
#3923 = DIRECTION ( 'NONE',  ( -0.000000000000000000, -0.000000000000000000, -1.000000000000000000 ) ) ;
#3924 = ORIENTED_EDGE ( 'NONE', *, *, #4581, .F. ) ;
#3925 = EDGE_CURVE ( 'NONE', #3208, #4113, #2207, .T. ) ;
#3926 = ADVANCED_FACE ( 'NONE', ( #4728 ), #5285, .F. ) ;
#3927 = PLANE ( 'NONE',  #587 ) ;
#3928 = CARTESIAN_POINT ( 'NONE',  ( 0.000000000000000000, 0.000000000000000000, 47.00000000000000000 ) ) ;
#3929 = DIRECTION ( 'NONE',  ( -0.000000000000000000, -0.000000000000000000, -1.000000000000000000 ) ) ;
#3930 = EDGE_CURVE ( 'NONE', #336, #5616, #4237, .T. ) ;
#3931 = LINE ( 'NONE', #580, #5463 ) ;
#3932 = ORIENTED_EDGE ( 'NONE', *, *, #5706, .F. ) ;
#3933 = EDGE_CURVE ( 'NONE', #4645, #2995, #5258, .T. ) ;
#3934 = CYLINDRICAL_SURFACE ( 'NONE', #4191, 19.00000000000000000 ) ;
#3935 = DIRECTION ( 'NONE',  ( -0.000000000000000000, -0.000000000000000000, -1.000000000000000000 ) ) ;
#3936 = EDGE_CURVE ( 'NONE', #1346, #554, #5154, .T. ) ;
#3937 = CARTESIAN_POINT ( 'NONE',  ( -12.84176997259613096, 28.64101934588367371, 2.395886979664402006 ) ) ;
#3938 = DIRECTION ( 'NONE',  ( -0.000000000000000000, -0.000000000000000000, -1.000000000000000000 ) ) ;
#3939 = ORIENTED_EDGE ( 'NONE', *, *, #1247, .T. ) ;
#3940 =( LENGTH_UNIT ( ) NAMED_UNIT ( * ) SI_UNIT ( .MILLI., .METRE. ) );
#3941 = CARTESIAN_POINT ( 'NONE',  ( 12.41746183822997551, 30.39531364385071655, 9.999999999999991118 ) ) ;
#3942 = DIRECTION ( 'NONE',  ( -1.000000000000000000, 0.000000000000000000, 0.000000000000000000 ) ) ;
#3943 = EDGE_CURVE ( 'NONE', #4451, #1278, #1727, .T. ) ;
#3944 = DIRECTION ( 'NONE',  ( -0.000000000000000000, -0.000000000000000000, 1.000000000000000000 ) ) ;
#3945 = AXIS2_PLACEMENT_3D ( 'NONE', #2218, #4179, #2803 ) ;
#3946 = CARTESIAN_POINT ( 'NONE',  ( 0.000000000000000000, 69.00000000000000000, 110.0000000000000000 ) ) ;
#3947 = CARTESIAN_POINT ( 'NONE',  ( -16.23652742703190199, -37.28747423195189015, -65.00000000000000000 ) ) ;
#3948 = VERTEX_POINT ( 'NONE', #3764 ) ;
#3949 = VERTEX_POINT ( 'NONE', #3697 ) ;
#3950 = ORIENTED_EDGE ( 'NONE', *, *, #3129, .F. ) ;
#3951 = ORIENTED_EDGE ( 'NONE', *, *, #4000, .T. ) ;
#3952 = CARTESIAN_POINT ( 'NONE',  ( 12.89959272829392845, 28.40844700521621036, 2.518705683379065974 ) ) ;
#3953 = DIRECTION ( 'NONE',  ( 1.000000000000000000, 0.000000000000000000, 0.000000000000000000 ) ) ;
#3954 = CARTESIAN_POINT ( 'NONE',  ( 8.983986218495337184, -23.34169575125378771, 7.586426789398496240 ) ) ;
#3955 = VERTEX_POINT ( 'NONE', #4787 ) ;
#3956 = CARTESIAN_POINT ( 'NONE',  ( -128.6881948289521631, 102.2453362568706865, 162.8064542903199765 ) ) ;
#3957 = CARTESIAN_POINT ( 'NONE',  ( -7.058581574212176690, -21.89022081680645826, 29.23014371996821481 ) ) ;
#3958 = EDGE_CURVE ( 'NONE', #453, #2206, #5311, .T. ) ;
#3959 = PLANE ( 'NONE',  #1230 ) ;
#3960 = ORIENTED_EDGE ( 'NONE', *, *, #1253, .F. ) ;
#3961 = CARTESIAN_POINT ( 'NONE',  ( 0.000000000000000000, 0.000000000000000000, 47.00000000000000000 ) ) ;
#3962 = FACE_OUTER_BOUND ( 'NONE', #4725, .T. ) ;
#3963 = CARTESIAN_POINT ( 'NONE',  ( 197.0000000000000000, 68.99999999999997158, 0.000000000000000000 ) ) ;
#3964 = DIRECTION ( 'NONE',  ( -1.000000000000000000, 0.000000000000000000, 0.000000000000000000 ) ) ;
#3965 = VERTEX_POINT ( 'NONE', #806 ) ;
#3966 = CARTESIAN_POINT ( 'NONE',  ( -25.00000000000000000, 0.000000000000000000, 50.00000000000000711 ) ) ;
#3967 = CIRCLE ( 'NONE', #4265, 23.00000000000000000 ) ;
#3968 = CARTESIAN_POINT ( 'NONE',  ( -5.116921499885075164, 22.42580359959007552, 37.27629952662707069 ) ) ;
#3969 = CIRCLE ( 'NONE', #4577, 24.99999999999999289 ) ;
#3970 = PLANE ( 'NONE',  #5993 ) ;
#3971 = CARTESIAN_POINT ( 'NONE',  ( -8.000000000000021316, 2.721075280251214820E-15, 1.999999999999986233 ) ) ;
#3972 = DIRECTION ( 'NONE',  ( -1.000000000000000000, 0.000000000000000000, 0.000000000000000000 ) ) ;
#3973 = EDGE_LOOP ( 'NONE', ( #5553, #4330, #519, #807, #5087, #5901 ) ) ;
#3974 = EDGE_LOOP ( 'NONE', ( #2759, #3960, #1643, #614 ) ) ;
#3975 = AXIS2_PLACEMENT_3D ( 'NONE', #4951, #546, #1561 ) ;
#3976 = AXIS2_PLACEMENT_3D ( 'NONE', #484, #2887, #4856 ) ;
#3977 = CARTESIAN_POINT ( 'NONE',  ( 13.30660938351089584, 26.80958678890347713, 4.207676383415306809 ) ) ;
#3978 = DIRECTION ( 'NONE',  ( -1.000000000000000000, 0.000000000000000000, 0.000000000000000000 ) ) ;
#3979 = CARTESIAN_POINT ( 'NONE',  ( -2.985931097914281462, -24.82479382442820537, 9.752995572818681680 ) ) ;
#3980 = ORIENTED_EDGE ( 'NONE', *, *, #2280, .T. ) ;
#3981 = AXIS2_PLACEMENT_3D ( 'NONE', #3946, #5949, #3491 ) ;
#3982 = CARTESIAN_POINT ( 'NONE',  ( -4.781067518356564072, -22.50057576469317411, 37.57069195157705366 ) ) ;
#3983 = CARTESIAN_POINT ( 'NONE',  ( -6.500000000000000000, 7.960204194457795477E-16, 1.000000000000000888 ) ) ;
#3984 = ORIENTED_EDGE ( 'NONE', *, *, #1058, .T. ) ;
#3985 = DIRECTION ( 'NONE',  ( 0.000000000000000000, 0.000000000000000000, 1.000000000000000000 ) ) ;
#3986 = VECTOR ( 'NONE', #2151, 1000.000000000000000 ) ;
#3987 = DIRECTION ( 'NONE',  ( -0.000000000000000000, -0.000000000000000000, 1.000000000000000000 ) ) ;
#3988 = DIRECTION ( 'NONE',  ( 0.000000000000000000, 0.000000000000000000, 1.000000000000000000 ) ) ;
#3989 = CARTESIAN_POINT ( 'NONE',  ( -44.00000000000000000, -13.41640786499873350, -45.00000000000000000 ) ) ;
#3990 = ORIENTED_EDGE ( 'NONE', *, *, #5817, .F. ) ;
#3991 = EDGE_CURVE ( 'NONE', #414, #4976, #532, .T. ) ;
#3992 = DIRECTION ( 'NONE',  ( 1.000000000000000000, 0.000000000000000000, 0.000000000000000000 ) ) ;
#3993 = CARTESIAN_POINT ( 'NONE',  ( -0.8980764441730644254, 22.98681745009828248, 24.31513574047610504 ) ) ;
#3994 = EDGE_CURVE ( 'NONE', #4815, #4122, #3239, .T. ) ;
#3995 = CARTESIAN_POINT ( 'NONE',  ( 0.000000000000000000, 0.000000000000000000, -110.0000000000000000 ) ) ;
#3996 = AXIS2_PLACEMENT_3D ( 'NONE', #3165, #5077, #4190 ) ;
#3997 = LINE ( 'NONE', #5514, #1026 ) ;
#3998 = ORIENTED_EDGE ( 'NONE', *, *, #5716, .T. ) ;
#3999 = ORIENTED_EDGE ( 'NONE', *, *, #1330, .F. ) ;
#4000 = EDGE_CURVE ( 'NONE', #3812, #5753, #2792, .T. ) ;
#4001 = EDGE_LOOP ( 'NONE', ( #1407, #1618, #4208, #2584 ) ) ;
#4002 = VECTOR ( 'NONE', #177, 1000.000000000000000 ) ;
#4003 = CARTESIAN_POINT ( 'NONE',  ( 13.19762691892552908, 27.23125096863189754, 3.538843351020406480 ) ) ;
#4004 = DIRECTION ( 'NONE',  ( 1.000000000000000000, 0.000000000000000000, 0.000000000000000000 ) ) ;
#4005 = ADVANCED_FACE ( 'NONE', ( #5799 ), #897, .T. ) ;
#4006 = DIRECTION ( 'NONE',  ( 0.000000000000000000, 0.000000000000000000, 1.000000000000000000 ) ) ;
#4007 = ORIENTED_EDGE ( 'NONE', *, *, #1732, .T. ) ;
#4008 = PRODUCT_RELATED_PRODUCT_CATEGORY ( 'part', '', ( #1222 ) ) ;
#4009 = ADVANCED_FACE ( 'NONE', ( #870 ), #385, .T. ) ;
#4010 = AXIS2_PLACEMENT_3D ( 'NONE', #1307, #2716, #3827 ) ;
#4011 = EDGE_CURVE ( 'NONE', #3367, #3955, #2845, .T. ) ;
#4012 = DIRECTION ( 'NONE',  ( -0.000000000000000000, 0.000000000000000000, -1.000000000000000000 ) ) ;
#4013 = EDGE_CURVE ( 'NONE', #2940, #1460, #1830, .T. ) ;
#4014 = DIRECTION ( 'NONE',  ( -7.939228591060055989E-17, -0.9872917187776014680, -0.1589184131344427708 ) ) ;
#4015 = CARTESIAN_POINT ( 'NONE',  ( 0.000000000000000000, 25.00000000000000000, -20.00000000000000000 ) ) ;
#4016 = ORIENTED_EDGE ( 'NONE', *, *, #40, .F. ) ;
#4017 = VERTEX_POINT ( 'NONE', #2340 ) ;
#4018 = LINE ( 'NONE', #198, #4051 ) ;
#4019 = B_SPLINE_CURVE_WITH_KNOTS ( 'NONE', 3,
 ( #850, #2802, #4312, #1810, #3777, #4772 ),
 .UNSPECIFIED., .F., .F.,
 ( 4, 2, 4 ),
 ( 0.002032958594636732723, 0.003043324567219493192, 0.004053690539802253662 ),
 .UNSPECIFIED. ) ;
#4020 = CARTESIAN_POINT ( 'NONE',  ( 64.99991398172927859, 76.99999716619419132, 1.734723475976807094E-15 ) ) ;
#4021 = AXIS2_PLACEMENT_3D ( 'NONE', #5218, #5739, #1214 ) ;
#4022 = DIRECTION ( 'NONE',  ( -0.000000000000000000, -0.000000000000000000, 1.000000000000000000 ) ) ;
#4023 = ORIENTED_EDGE ( 'NONE', *, *, #1937, .T. ) ;
#4024 = LINE ( 'NONE', #3574, #3606 ) ;
#4025 = CARTESIAN_POINT ( 'NONE',  ( 0.9006954679665252206, 22.98346407483541753, 24.32584948309267148 ) ) ;
#4026 = LINE ( 'NONE', #540, #3364 ) ;
#4027 = DIRECTION ( 'NONE',  ( 1.000000000000000000, 0.000000000000000000, 0.000000000000000000 ) ) ;
#4028 = ORIENTED_EDGE ( 'NONE', *, *, #2769, .T. ) ;
#4029 = ORIENTED_EDGE ( 'NONE', *, *, #4859, .F. ) ;
#4030 = ORIENTED_EDGE ( 'NONE', *, *, #1326, .F. ) ;
#4031 = CARTESIAN_POINT ( 'NONE',  ( 18.00000000000001421, 30.39531364385072010, 5.999999999999990230 ) ) ;
#4032 = FACE_OUTER_BOUND ( 'NONE', #5293, .T. ) ;
#4033 = LINE ( 'NONE', #1100, #2865 ) ;
#4034 = LINE ( 'NONE', #1931, #5115 ) ;
#4035 = CARTESIAN_POINT ( 'NONE',  ( 0.000000000000000000, 0.000000000000000000, -248.0000000000000000 ) ) ;
#4036 = ORIENTED_EDGE ( 'NONE', *, *, #4833, .T. ) ;
#4037 =( NAMED_UNIT ( * ) SI_UNIT ( $, .STERADIAN. ) SOLID_ANGLE_UNIT ( ) );
#4038 = CARTESIAN_POINT ( 'NONE',  ( -5.121424986093042087, -22.42477833501277829, 37.27216187635247024 ) ) ;
#4039 = CYLINDRICAL_SURFACE ( 'NONE', #4734, 6.500000000000001776 ) ;
#4040 = ORIENTED_EDGE ( 'NONE', *, *, #4152, .F. ) ;
#4041 = MECHANICAL_DESIGN_GEOMETRIC_PRESENTATION_REPRESENTATION (  '', ( #5447 ), #5133 ) ;
#4042 = CARTESIAN_POINT ( 'NONE',  ( 0.000000000000000000, 0.000000000000000000, 39.00000000000001421 ) ) ;
#4043 = DIRECTION ( 'NONE',  ( 0.000000000000000000, 0.000000000000000000, 1.000000000000000000 ) ) ;
#4044 = CARTESIAN_POINT ( 'NONE',  ( 19.00000000000000000, 0.000000000000000000, -248.0000000000000000 ) ) ;
#4045 = ORIENTED_EDGE ( 'NONE', *, *, #6217, .F. ) ;
#4046 = CARTESIAN_POINT ( 'NONE',  ( 0.4786673552078670735, 22.99919074915722916, 9.998953803578743305 ) ) ;
#4047 = LINE ( 'NONE', #2671, #1655 ) ;
#4048 = CARTESIAN_POINT ( 'NONE',  ( -2.223777455422794702, 22.89327810718596368, 24.60873847605252251 ) ) ;
#4049 = CARTESIAN_POINT ( 'NONE',  ( 6.685354258535094907, 24.10283321907682108, 8.717551967824453740 ) ) ;
#4050 = CARTESIAN_POINT ( 'NONE',  ( 0.000000000000000000, 0.000000000000000000, -175.0000000000000000 ) ) ;
#4051 = VECTOR ( 'NONE', #164, 1000.000000000000000 ) ;
#4052 = ORIENTED_EDGE ( 'NONE', *, *, #4952, .F. ) ;
#4053 = ORIENTED_EDGE ( 'NONE', *, *, #463, .T. ) ;
#4054 = AXIS2_PLACEMENT_3D ( 'NONE', #4203, #1792, #3692 ) ;
#4055 = EDGE_LOOP ( 'NONE', ( #1840, #3597, #1132, #761 ) ) ;
#4056 = CARTESIAN_POINT ( 'NONE',  ( 8.000000000000000000, 110.3953136438507130, 12.00000000000000000 ) ) ;
#4057 = DIRECTION ( 'NONE',  ( -0.000000000000000000, -0.000000000000000000, -1.000000000000000000 ) ) ;
#4058 = EDGE_CURVE ( 'NONE', #5299, #2249, #2371, .T. ) ;
#4059 = CARTESIAN_POINT ( 'NONE',  ( 23.00000000000000000, 2.816687638038912352E-15, 39.00000000000001421 ) ) ;
#4060 = CARTESIAN_POINT ( 'NONE',  ( 172.0000000000000000, 68.99999999999998579, 110.0000000000000000 ) ) ;
#4061 = FACE_OUTER_BOUND ( 'NONE', #5829, .T. ) ;
#4062 = EDGE_LOOP ( 'NONE', ( #1558, #2427, #729, #5814 ) ) ;
#4063 = ADVANCED_FACE ( 'NONE', ( #3207 ), #286, .T. ) ;
#4064 = EDGE_CURVE ( 'NONE', #997, #1301, #1959, .T. ) ;
#4065 = APPLICATION_PROTOCOL_DEFINITION ( 'draft international standard', 'automotive_design', 1998, #1590 ) ;
#4066 = CARTESIAN_POINT ( 'NONE',  ( 1.908796811648538206E-15, -20.00000000000000711, 39.27501000028011902 ) ) ;
#4067 = CIRCLE ( 'NONE', #5217, 17.00000000000000000 ) ;
#4068 = ADVANCED_FACE ( 'NONE', ( #2434, #6312 ), #1050, .T. ) ;
#4069 = ORIENTED_EDGE ( 'NONE', *, *, #5716, .F. ) ;
#4070 = CARTESIAN_POINT ( 'NONE',  ( 212.0000000000000284, 68.99999999999997158, 0.000000000000000000 ) ) ;
#4071 = ORIENTED_EDGE ( 'NONE', *, *, #5533, .F. ) ;
#4072 = EDGE_CURVE ( 'NONE', #5649, #371, #4817, .T. ) ;
#4073 = ADVANCED_FACE ( 'NONE', ( #3366 ), #2041, .T. ) ;
#4074 = AXIS2_PLACEMENT_3D ( 'NONE', #3018, #4983, #5928 ) ;
#4075 = DIRECTION ( 'NONE',  ( 0.000000000000000000, 0.000000000000000000, -1.000000000000000000 ) ) ;
#4076 = CARTESIAN_POINT ( 'NONE',  ( 0.000000000000000000, 0.000000000000000000, 0.000000000000000000 ) ) ;
#4077 = DIRECTION ( 'NONE',  ( 1.000000000000000000, 0.000000000000000000, 0.000000000000000000 ) ) ;
#4078 = DIRECTION ( 'NONE',  ( -0.000000000000000000, -0.000000000000000000, -1.000000000000000000 ) ) ;
#4079 = EDGE_LOOP ( 'NONE', ( #2644, #2496, #4197, #269 ) ) ;
#4080 = DIRECTION ( 'NONE',  ( 0.000000000000000000, 0.000000000000000000, 1.000000000000000000 ) ) ;
#4081 =( NAMED_UNIT ( * ) SI_UNIT ( $, .STERADIAN. ) SOLID_ANGLE_UNIT ( ) );
#4082 = CARTESIAN_POINT ( 'NONE',  ( 6.703552034654557623, 22.00169986843530268, 28.40415011795442979 ) ) ;
#4083 = ADVANCED_FACE ( 'NONE', ( #4919, #3431 ), #518, .T. ) ;
#4084 = CARTESIAN_POINT ( 'NONE',  ( -15.63375151319036682, 19.51424150167564520, 0.7397720130343804490 ) ) ;
#4085 = CYLINDRICAL_SURFACE ( 'NONE', #3083, 6.500000000000001776 ) ;
#4086 = CIRCLE ( 'NONE', #5348, 17.00000000000000000 ) ;
#4087 = EDGE_LOOP ( 'NONE', ( #5000, #4431, #813, #2950 ) ) ;
#4088 = EDGE_LOOP ( 'NONE', ( #2100, #3642, #5515, #4686, #5096, #1094 ) ) ;
#4089 = CARTESIAN_POINT ( 'NONE',  ( 0.000000000000000000, 0.000000000000000000, 276.0000000000000000 ) ) ;
#4090 = VECTOR ( 'NONE', #2338, 1000.000000000000000 ) ;
#4091 = PRODUCT_DEFINITION_SHAPE ( 'NONE', 'NONE',  #6367 ) ;
#4092 = CARTESIAN_POINT ( 'NONE',  ( -6.500000000000000000, 0.000000000000000000, 0.000000000000000000 ) ) ;
#4093 = DIRECTION ( 'NONE',  ( 1.000000000000000000, 0.000000000000000000, 0.000000000000000000 ) ) ;
#4094 = CARTESIAN_POINT ( 'NONE',  ( 44.00000000000000000, -13.41640786499874771, -240.0000000000000000 ) ) ;
#4095 = AXIS2_PLACEMENT_3D ( 'NONE', #5079, #1684, #668 ) ;
#4096 = CARTESIAN_POINT ( 'NONE',  ( -15.99408614349810698, -19.21429697996681440, -4.336808689942017736E-15 ) ) ;
#4097 = ORIENTED_EDGE ( 'NONE', *, *, #660, .F. ) ;
#4098 = EDGE_CURVE ( 'NONE', #5753, #4162, #5754, .T. ) ;
#4099 = ITEM_DEFINED_TRANSFORMATION ( 'NONE', 'NONE', #2954,  #6349 ) ;
#4100 = CIRCLE ( 'NONE', #528, 90.00000000000000000 ) ;
#4101 = CONTEXT_DEPENDENT_SHAPE_REPRESENTATION ( #1852, #5597 ) ;
#4102 = CARTESIAN_POINT ( 'NONE',  ( 17.05141243254543681, -12.25762350764760455, 12.00000000000000000 ) ) ;
#4103 = EDGE_CURVE ( 'NONE', #1346, #5357, #64, .T. ) ;
#4104 = ADVANCED_FACE ( 'NONE', ( #4523 ), #185, .F. ) ;
#4105 = ORIENTED_EDGE ( 'NONE', *, *, #5064, .T. ) ;
#4106 = PLANE ( 'NONE',  #321 ) ;
#4107 = EDGE_LOOP ( 'NONE', ( #3053, #1434, #2770, #711 ) ) ;
#4108 = CYLINDRICAL_SURFACE ( 'NONE', #1695, 90.00000000000321165 ) ;
#4109 = DIRECTION ( 'NONE',  ( 1.000000000000000000, 0.000000000000000000, -0.000000000000000000 ) ) ;
#4110 = ADVANCED_FACE ( 'NONE', ( #4061 ), #573, .T. ) ;
#4111 = DIRECTION ( 'NONE',  ( 0.000000000000000000, 0.000000000000000000, 1.000000000000000000 ) ) ;
#4112 = CARTESIAN_POINT ( 'NONE',  ( 2.012341796004660122, -19.89850447888114005, 39.00000000000001421 ) ) ;
#4113 = VERTEX_POINT ( 'NONE', #6048 ) ;
#4114 = CIRCLE ( 'NONE', #5053, 17.00000000000000000 ) ;
#4115 = DIRECTION ( 'NONE',  ( -0.000000000000000000, -0.000000000000000000, -1.000000000000000000 ) ) ;
#4116 = CARTESIAN_POINT ( 'NONE',  ( 7.071085268539269109, 21.88683845148715079, 34.31457501568616664 ) ) ;
#4117 = CIRCLE ( 'NONE', #3513, 90.00000000000319744 ) ;
#4118 = CARTESIAN_POINT ( 'NONE',  ( -5.542644329336979148, 24.38138258431391847, 9.119897054702294170 ) ) ;
#4119 = CARTESIAN_POINT ( 'NONE',  ( 6.135028333862784677, -22.16704433745741554, 36.09490741883096376 ) ) ;
#4120 = VERTEX_POINT ( 'NONE', #5592 ) ;
#4121 = ORIENTED_EDGE ( 'NONE', *, *, #5749, .F. ) ;
#4122 = VERTEX_POINT ( 'NONE', #4128 ) ;
#4123 = DIRECTION ( 'NONE',  ( 0.000000000000000000, 0.000000000000000000, -1.000000000000000000 ) ) ;
#4124 = EDGE_CURVE ( 'NONE', #1758, #6160, #406, .T. ) ;
#4125 = CARTESIAN_POINT ( 'NONE',  ( -2.385244779468109755E-15, -1.040834085586084257E-14, -110.0000000000000000 ) ) ;
#4126 = LINE ( 'NONE', #6133, #309 ) ;
#4127 = DIRECTION ( 'NONE',  ( -0.000000000000000000, -0.000000000000000000, 1.000000000000000000 ) ) ;
#4128 = CARTESIAN_POINT ( 'NONE',  ( 17.00000000000000000, 25.00000000000000355, -225.0000000000000000 ) ) ;
#4129 = ORIENTED_EDGE ( 'NONE', *, *, #3601, .F. ) ;
#4130 = CARTESIAN_POINT ( 'NONE',  ( 0.8355139846970627282, -23.00151096327411793, 10.00195343045036189 ) ) ;
#4131 = AXIS2_PLACEMENT_3D ( 'NONE', #5332, #1947, #982 ) ;
#4132 = ORIENTED_EDGE ( 'NONE', *, *, #5426, .F. ) ;
#4133 = CARTESIAN_POINT ( 'NONE',  ( 0.000000000000000000, 120.0000000000000000, 12.00000000000000000 ) ) ;
#4134 = ORIENTED_EDGE ( 'NONE', *, *, #1593, .F. ) ;
#4135 =( REPRESENTATION_RELATIONSHIP ('NONE','NONE', #632, #5606 ) REPRESENTATION_RELATIONSHIP_WITH_TRANSFORMATION ( #930 )SHAPE_REPRESENTATION_RELATIONSHIP( ) );
#4136 = LINE ( 'NONE', #5575, #3826 ) ;
#4137 = EDGE_CURVE ( 'NONE', #4340, #2231, #3080, .T. ) ;
#4138 = CARTESIAN_POINT ( 'NONE',  ( 3.122849337825750617E-15, -17.00000000000000000, 301.0000000000000568 ) ) ;
#4139 = CARTESIAN_POINT ( 'NONE',  ( 0.000000000000000000, 0.000000000000000000, 0.000000000000000000 ) ) ;
#4140 = VERTEX_POINT ( 'NONE', #1170 ) ;
#4141 = CARTESIAN_POINT ( 'NONE',  ( 19.00000000000000000, 2.326828918379970970E-15, 15.00000000000000000 ) ) ;
#4142 = PRODUCT_DEFINITION_SHAPE ( 'NONE', 'NONE',  #6375 ) ;
#4143 = CARTESIAN_POINT ( 'NONE',  ( 0.000000000000000000, 0.000000000000000000, -273.0000000000000000 ) ) ;
#4144 = CARTESIAN_POINT ( 'NONE',  ( -8.000000000000005329, 110.3953136438506988, 0.000000000000000000 ) ) ;
#4145 = PRODUCT_DEFINITION_FORMATION_WITH_SPECIFIED_SOURCE ( 'ANY', '', #1222, .NOT_KNOWN. ) ;
#4146 = ADVANCED_FACE ( 'NONE', ( #1103 ), #2137, .T. ) ;
#4147 = LINE ( 'NONE', #6036, #2230 ) ;
#4148 = CYLINDRICAL_SURFACE ( 'NONE', #5876, 89.87058297576892585 ) ;
#4149 = ORIENTED_EDGE ( 'NONE', *, *, #5024, .F. ) ;
#4150 = ORIENTED_EDGE ( 'NONE', *, *, #3425, .T. ) ;
#4151 = CARTESIAN_POINT ( 'NONE',  ( -15.82602517378898987, 37.28747423195201094, 15.00000000000000000 ) ) ;
#4152 = EDGE_CURVE ( 'NONE', #2750, #5198, #3135, .T. ) ;
#4153 = EDGE_CURVE ( 'NONE', #1758, #738, #5495, .T. ) ;
#4154 = DIRECTION ( 'NONE',  ( 0.000000000000000000, 0.000000000000000000, -1.000000000000000000 ) ) ;
#4155 = DIRECTION ( 'NONE',  ( 1.000000000000000000, 0.000000000000000000, 0.000000000000000000 ) ) ;
#4156 = FACE_OUTER_BOUND ( 'NONE', #5489, .T. ) ;
#4157 = ORIENTED_EDGE ( 'NONE', *, *, #5812, .F. ) ;
#4158 = PLANE ( 'NONE',  #1719 ) ;
#4159 = VERTEX_POINT ( 'NONE', #6081 ) ;
#4160 = LINE ( 'NONE', #3624, #5139 ) ;
#4161 = CARTESIAN_POINT ( 'NONE',  ( 14.34541152806172626, -17.98734769216428830, 2.761683449857409656 ) ) ;
#4162 = VERTEX_POINT ( 'NONE', #2619 ) ;
#4163 = DIRECTION ( 'NONE',  ( -0.000000000000000000, -0.000000000000000000, 1.000000000000000000 ) ) ;
#4164 = ORIENTED_EDGE ( 'NONE', *, *, #5548, .T. ) ;
#4165 = AXIS2_PLACEMENT_3D ( 'NONE', #6203, #4582, #1783 ) ;
#4166 = AXIS2_PLACEMENT_3D ( 'NONE', #3855, #2850, #1478 ) ;
#4167 = VECTOR ( 'NONE', #2416, 1000.000000000000000 ) ;
#4168 = UNCERTAINTY_MEASURE_WITH_UNIT (LENGTH_MEASURE( 1.000000000000000082E-05 ), #1280, 'distance_accuracy_value', 'NONE');
#4169 = DIRECTION ( 'NONE',  ( 1.000000000000000000, 0.000000000000000000, 0.000000000000000000 ) ) ;
#4170 = CARTESIAN_POINT ( 'NONE',  ( 0.000000000000000000, 0.000000000000000000, -115.0000000000000000 ) ) ;
#4171 = PLANE ( 'NONE',  #1421 ) ;
#4172 = CARTESIAN_POINT ( 'NONE',  ( 0.000000000000000000, 0.000000000000000000, 39.00000000000001421 ) ) ;
#4173 = ORIENTED_EDGE ( 'NONE', *, *, #6105, .F. ) ;
#4174 =( GEOMETRIC_REPRESENTATION_CONTEXT ( 3 ) GLOBAL_UNCERTAINTY_ASSIGNED_CONTEXT ( ( #136 ) ) GLOBAL_UNIT_ASSIGNED_CONTEXT ( ( #2437, #449, #6315 ) ) REPRESENTATION_CONTEXT ( 'NONE', 'WORKASPACE' ) );
#4175 = CARTESIAN_POINT ( 'NONE',  ( -15.99408614349810698, 16.52843635781563592, 0.000000000000000000 ) ) ;
#4176 = ORIENTED_EDGE ( 'NONE', *, *, #2870, .T. ) ;
#4177 = ADVANCED_FACE ( 'NONE', ( #1660 ), #4622, .T. ) ;
#4178 = CARTESIAN_POINT ( 'NONE',  ( 2.426466830553629439, 24.88612820222271438, 38.88851386838336310 ) ) ;
#4179 = DIRECTION ( 'NONE',  ( 0.000000000000000000, 0.000000000000000000, -1.000000000000000000 ) ) ;
#4180 = AXIS2_PLACEMENT_3D ( 'NONE', #4848, #312, #858 ) ;
#4181 = EDGE_CURVE ( 'NONE', #4348, #4113, #3272, .T. ) ;
#4182 = CARTESIAN_POINT ( 'NONE',  ( 14.33006727100665856, 20.49285708348135415, 2.782958588747960427 ) ) ;
#4183 = CARTESIAN_POINT ( 'NONE',  ( 7.471932569767337995, -21.75248695045747382, 32.56440574765390039 ) ) ;
#4184 = EDGE_CURVE ( 'NONE', #161, #5556, #5337, .T. ) ;
#4185 = ORIENTED_EDGE ( 'NONE', *, *, #108, .F. ) ;
#4186 = ORIENTED_EDGE ( 'NONE', *, *, #865, .T. ) ;
#4187 = CIRCLE ( 'NONE', #6150, 1.000000000000000888 ) ;
#4188 = CARTESIAN_POINT ( 'NONE',  ( 2.546401178541497462E-16, 25.00000000000000000, 24.27501000028010125 ) ) ;
#4189 = CARTESIAN_POINT ( 'NONE',  ( 0.000000000000000000, 0.000000000000000000, 0.000000000000000000 ) ) ;
#4190 = DIRECTION ( 'NONE',  ( -1.000000000000000000, 0.000000000000000000, 0.000000000000000000 ) ) ;
#4191 = AXIS2_PLACEMENT_3D ( 'NONE', #5450, #3441, #1031 ) ;
#4192 = ADVANCED_FACE ( 'NONE', ( #2594 ), #156, .F. ) ;
#4193 = FACE_OUTER_BOUND ( 'NONE', #1482, .T. ) ;
#4194 = ADVANCED_FACE ( 'NONE', ( #613 ), #2049, .T. ) ;
#4195 = VERTEX_POINT ( 'NONE', #5080 ) ;
#4196 = DIRECTION ( 'NONE',  ( 1.852483853906148040E-16, 1.000000000000000000, 0.000000000000000000 ) ) ;
#4197 = ORIENTED_EDGE ( 'NONE', *, *, #3066, .T. ) ;
#4198 = COLOUR_RGB ( '',0.7921568627450980005, 0.8196078431372548767, 0.9333333333333333481 ) ;
#4199 = AXIS2_PLACEMENT_3D ( 'NONE', #3197, #5203, #4093 ) ;
#4200 = CARTESIAN_POINT ( 'NONE',  ( 44.56092774862622719, -29.44644455561813956, 15.00000000000000000 ) ) ;
#4201 = EDGE_CURVE ( 'NONE', #5742, #2595, #672, .T. ) ;
#4202 = ITEM_DEFINED_TRANSFORMATION ( 'NONE', 'NONE', #6250,  #6349 ) ;
#4203 = CARTESIAN_POINT ( 'NONE',  ( 0.000000000000000000, 0.000000000000000000, 16.00000000000000000 ) ) ;
#4204 = CIRCLE ( 'NONE', #5653, 17.00000000000000000 ) ;
#4205 = ORIENTED_EDGE ( 'NONE', *, *, #4345, .T. ) ;
#4206 = VECTOR ( 'NONE', #438, 1000.000000000000000 ) ;
#4207 = CARTESIAN_POINT ( 'NONE',  ( 0.000000000000000000, 0.000000000000000000, 0.000000000000000000 ) ) ;
#4208 = ORIENTED_EDGE ( 'NONE', *, *, #1367, .F. ) ;
#4209 = CIRCLE ( 'NONE', #215, 22.67164836619068424 ) ;
#4210 = DIRECTION ( 'NONE',  ( -1.000000000000000000, 0.000000000000000000, 0.000000000000000000 ) ) ;
#4211 = EDGE_CURVE ( 'NONE', #4844, #760, #1313, .T. ) ;
#4212 =( LENGTH_UNIT ( ) NAMED_UNIT ( * ) SI_UNIT ( .MILLI., .METRE. ) );
#4213 = CARTESIAN_POINT ( 'NONE',  ( 17.00000000000000000, 0.000000000000000000, -45.00000000000000000 ) ) ;
#4214 = DIRECTION ( 'NONE',  ( -1.852483853906148040E-16, -1.000000000000000000, -1.239088197126290570E-16 ) ) ;
#4215 = VECTOR ( 'NONE', #2056, 1000.000000000000000 ) ;
#4216 = FACE_OUTER_BOUND ( 'NONE', #413, .T. ) ;
#4217 = ORIENTED_EDGE ( 'NONE', *, *, #4268, .F. ) ;
#4218 = CYLINDRICAL_SURFACE ( 'NONE', #1321, 46.00000000000000000 ) ;
#4219 = EDGE_LOOP ( 'NONE', ( #929, #2688, #3951, #2841, #6084 ) ) ;
#4220 = CARTESIAN_POINT ( 'NONE',  ( 14.00000000000000000, 14.00000000000000000, 0.000000000000000000 ) ) ;
#4221 = DIRECTION ( 'NONE',  ( -1.000000000000000000, 0.000000000000000000, 0.000000000000000000 ) ) ;
#4222 = DIRECTION ( 'NONE',  ( 0.000000000000000000, 0.000000000000000000, 1.000000000000000000 ) ) ;
#4223 = CIRCLE ( 'NONE', #3399, 17.00000000000000000 ) ;
#4224 = CIRCLE ( 'NONE', #2065, 166.8359700257217071 ) ;
#4225 = CARTESIAN_POINT ( 'NONE',  ( 4.955340051326921902, -24.50653216723388894, 37.42604413602553137 ) ) ;
#4226 = ORIENTED_EDGE ( 'NONE', *, *, #2393, .F. ) ;
#4227 = ORIENTED_EDGE ( 'NONE', *, *, #5078, .T. ) ;
#4228 = CARTESIAN_POINT ( 'NONE',  ( -3.765864371162154889, 24.71817793568963495, 25.27057431607724780 ) ) ;
#4229 = CARTESIAN_POINT ( 'NONE',  ( 21.00000000000000355, 2.571758278209442056E-15, 16.00000000000000000 ) ) ;
#4230 = CARTESIAN_POINT ( 'NONE',  ( 0.000000000000000000, 120.0000000000000000, -4.000000000000000000 ) ) ;
#4231 = DIRECTION ( 'NONE',  ( -0.000000000000000000, -0.000000000000000000, -1.000000000000000000 ) ) ;
#4232 = ORIENTED_EDGE ( 'NONE', *, *, #5705, .F. ) ;
#4233 = ORIENTED_EDGE ( 'NONE', *, *, #4400, .T. ) ;
#4234 = SHAPE_DEFINITION_REPRESENTATION ( #1744, #2313 ) ;
#4235 = DIRECTION ( 'NONE',  ( -0.000000000000000000, -0.000000000000000000, -1.000000000000000000 ) ) ;
#4236 = VERTEX_POINT ( 'NONE', #767 ) ;
#4237 = LINE ( 'NONE', #774, #6079 ) ;
#4238 = ORIENTED_EDGE ( 'NONE', *, *, #1241, .F. ) ;
#4239 = CARTESIAN_POINT ( 'NONE',  ( 0.000000000000000000, 0.000000000000000000, 281.0000000000000000 ) ) ;
#4240 = VECTOR ( 'NONE', #1819, 1000.000000000000000 ) ;
#4241 = LINE ( 'NONE', #2755, #227 ) ;
#4242 = FACE_OUTER_BOUND ( 'NONE', #4797, .T. ) ;
#4243 = CARTESIAN_POINT ( 'NONE',  ( -6.502944117165513127, -24.14103883855863941, 35.54306285688424794 ) ) ;
#4244 = EDGE_LOOP ( 'NONE', ( #2459, #5173 ) ) ;
#4245 = CARTESIAN_POINT ( 'NONE',  ( 0.000000000000000000, 0.000000000000000000, 301.0000000000000568 ) ) ;
#4246 = ORIENTED_EDGE ( 'NONE', *, *, #4756, .F. ) ;
#4247 = CARTESIAN_POINT ( 'NONE',  ( 7.019376005445150390, 23.99453911528665984, 29.12205218481382829 ) ) ;
#4248 = CARTESIAN_POINT ( 'NONE',  ( 2.876010458515648960, 22.82309565144259267, 38.71608687161452877 ) ) ;
#4249 = LINE ( 'NONE', #339, #2961 ) ;
#4250 = CARTESIAN_POINT ( 'NONE',  ( 5.958341177435918290, -24.28123298992124290, 27.19342269918141852 ) ) ;
#4251 = ORIENTED_EDGE ( 'NONE', *, *, #5986, .F. ) ;
#4252 = ORIENTED_EDGE ( 'NONE', *, *, #4013, .T. ) ;
#4253 = DIRECTION ( 'NONE',  ( 0.000000000000000000, 0.000000000000000000, 1.000000000000000000 ) ) ;
#4254 = PRODUCT_DEFINITION_FORMATION_WITH_SPECIFIED_SOURCE ( 'ANY', '', #2145, .NOT_KNOWN. ) ;
#4255 = CARTESIAN_POINT ( 'NONE',  ( 0.000000000000000000, 120.0000000000000000, 16.00000000000000000 ) ) ;
#4256 = DIRECTION ( 'NONE',  ( 0.000000000000000000, 0.000000000000000000, 1.000000000000000000 ) ) ;
#4257 = DIRECTION ( 'NONE',  ( 1.000000000000000000, 0.000000000000000000, 0.000000000000000000 ) ) ;
#4258 = ORIENTED_EDGE ( 'NONE', *, *, #5706, .T. ) ;
#4259 = ORIENTED_EDGE ( 'NONE', *, *, #47, .F. ) ;
#4260 = FACE_OUTER_BOUND ( 'NONE', #2138, .T. ) ;
#4261 = CARTESIAN_POINT ( 'NONE',  ( -12.41746183823000393, 30.39531364385071655, 9.999999999999991118 ) ) ;
#4262 = EDGE_LOOP ( 'NONE', ( #3581, #4232 ) ) ;
#4263 = CARTESIAN_POINT ( 'NONE',  ( 0.000000000000000000, 134.5953136438507158, 12.00000000000000000 ) ) ;
#4264 = ORIENTED_EDGE ( 'NONE', *, *, #1611, .F. ) ;
#4265 = AXIS2_PLACEMENT_3D ( 'NONE', #4042, #4075, #2090 ) ;
#4266 = EDGE_CURVE ( 'NONE', #5090, #4236, #4870, .T. ) ;
#4267 = CIRCLE ( 'NONE', #684, 7.500000000000000000 ) ;
#4268 = EDGE_CURVE ( 'NONE', #1077, #5299, #1272, .T. ) ;
#4269 = LINE ( 'NONE', #6248, #1401 ) ;
#4270 = EDGE_CURVE ( 'NONE', #5794, #5286, #2711, .T. ) ;
#4271 = DIRECTION ( 'NONE',  ( 1.000000000000000000, 0.000000000000000000, 0.000000000000000000 ) ) ;
#4272 = DIRECTION ( 'NONE',  ( -1.000000000000000000, 0.000000000000000000, 0.000000000000000000 ) ) ;
#4273 = CARTESIAN_POINT ( 'NONE',  ( -3.766262172602994340, -24.71811694763051293, 25.27080528860306430 ) ) ;
#4274 = ORIENTED_EDGE ( 'NONE', *, *, #6219, .T. ) ;
#4275 = EDGE_CURVE ( 'NONE', #116, #4754, #3686, .T. ) ;
#4276 = AXIS2_PLACEMENT_3D ( 'NONE', #917, #6235, #344 ) ;
#4277 = UNCERTAINTY_MEASURE_WITH_UNIT (LENGTH_MEASURE( 1.000000000000000082E-05 ), #4212, 'distance_accuracy_value', 'NONE');
#4278 = CARTESIAN_POINT ( 'NONE',  ( -43.99999999999990052, 13.41640786499905147, -175.0000000000000284 ) ) ;
#4279 = CARTESIAN_POINT ( 'NONE',  ( 0.4912064067414986801, 25.00000000000000711, 39.27501000028010480 ) ) ;
#4280 = CARTESIAN_POINT ( 'NONE',  ( 44.00000000000000000, -13.41640786499873705, -180.0000000000000000 ) ) ;
#4281 = CARTESIAN_POINT ( 'NONE',  ( 0.000000000000000000, 0.000000000000000000, 44.00000000000000711 ) ) ;
#4282 = AXIS2_PLACEMENT_3D ( 'NONE', #2474, #523, #4304 ) ;
#4283 = CARTESIAN_POINT ( 'NONE',  ( 5.640759563529097242, -24.35584729907773749, 36.72391480687588228 ) ) ;
#4284 = VERTEX_POINT ( 'NONE', #460 ) ;
#4285 = PRODUCT_RELATED_PRODUCT_CATEGORY ( 'part', '', ( #6067 ) ) ;
#4286 = EDGE_CURVE ( 'NONE', #5613, #6010, #4297, .T. ) ;
#4287 = ORIENTED_EDGE ( 'NONE', *, *, #327, .F. ) ;
#4288 = CARTESIAN_POINT ( 'NONE',  ( -6.830924868230225044, 24.04887075291641452, 34.88135594814352913 ) ) ;
#4289 = VECTOR ( 'NONE', #2518, 1000.000000000000000 ) ;
#4290 = CARTESIAN_POINT ( 'NONE',  ( 44.00000000000008527, 13.41640786499836224, -65.00000000000000000 ) ) ;
#4291 = CYLINDRICAL_SURFACE ( 'NONE', #4401, 17.00000000000000000 ) ;
#4292 = CARTESIAN_POINT ( 'NONE',  ( -44.64065620456596406, -28.99954194078535963, 0.000000000000000000 ) ) ;
#4293 = AXIS2_PLACEMENT_3D ( 'NONE', #778, #5670, #4272 ) ;
#4294 = ORIENTED_EDGE ( 'NONE', *, *, #707, .F. ) ;
#4295 = EDGE_LOOP ( 'NONE', ( #4468, #4611, #3232, #634 ) ) ;
#4296 = ORIENTED_EDGE ( 'NONE', *, *, #1596, .F. ) ;
#4297 = CIRCLE ( 'NONE', #913, 90.00000000000321165 ) ;
#4298 = CARTESIAN_POINT ( 'NONE',  ( 25.00000000000000000, 3.061616997868383043E-15, 0.000000000000000000 ) ) ;
#4299 = CYLINDRICAL_SURFACE ( 'NONE', #2658, 14.00000000000000000 ) ;
#4300 = CARTESIAN_POINT ( 'NONE',  ( 17.00000000000000000, 25.00000000000000355, -195.0000000000000000 ) ) ;
#4301 = EDGE_LOOP ( 'NONE', ( #5312, #5972, #5696, #80 ) ) ;
#4302 = AXIS2_PLACEMENT_3D ( 'NONE', #4638, #5063, #2184 ) ;
#4303 = AXIS2_PLACEMENT_3D ( 'NONE', #2136, #6080, #5622 ) ;
#4304 = DIRECTION ( 'NONE',  ( -2.634026558639406403E-17, 0.9868877816584149532, 0.1614078883243708906 ) ) ;
#4305 = CARTESIAN_POINT ( 'NONE',  ( 8.000000000000007105, 72.93807001241029297, 12.00000000000000000 ) ) ;
#4306 = CIRCLE ( 'NONE', #6274, 90.00000000000000000 ) ;
#4307 = DIRECTION ( 'NONE',  ( -0.000000000000000000, -0.000000000000000000, 1.000000000000000000 ) ) ;
#4308 = CARTESIAN_POINT ( 'NONE',  ( -5.133588784792095794, -24.46788053448571176, 26.30186172257456079 ) ) ;
#4309 = VERTEX_POINT ( 'NONE', #5330 ) ;
#4310 = CARTESIAN_POINT ( 'NONE',  ( 0.2052511266213280505, 21.25619793154159964, 15.00000000000000000 ) ) ;
#4311 = AXIS2_PLACEMENT_3D ( 'NONE', #2925, #4902, #559 ) ;
#4312 = CARTESIAN_POINT ( 'NONE',  ( -0.6815295361380612205, 19.99121204295638776, 39.25166565497248428 ) ) ;
#4313 = CARTESIAN_POINT ( 'NONE',  ( 2.012341796004660122, 19.89850447888114005, 39.00000000000001421 ) ) ;
#4314 = EDGE_CURVE ( 'NONE', #5880, #3234, #5144, .T. ) ;
#4315 = AXIS2_PLACEMENT_3D ( 'NONE', #3092, #2668, #3604 ) ;
#4316 = CARTESIAN_POINT ( 'NONE',  ( 197.0000000000000000, 68.99999999999997158, 110.0000000000000000 ) ) ;
#4317 = CARTESIAN_POINT ( 'NONE',  ( 5.474672603935804460, -24.39383812260185636, 36.90705202433115772 ) ) ;
#4318 = ORIENTED_EDGE ( 'NONE', *, *, #5437, .T. ) ;
#4319 = CARTESIAN_POINT ( 'NONE',  ( -44.64065620456893413, -28.99954194078699032, -180.0000000000000000 ) ) ;
#4320 = EDGE_LOOP ( 'NONE', ( #4350, #5793, #1788, #5134 ) ) ;
#4321 = AXIS2_PLACEMENT_3D ( 'NONE', #5214, #5185, #1374 ) ;
#4322 = DIRECTION ( 'NONE',  ( -0.000000000000000000, -0.000000000000000000, -1.000000000000000000 ) ) ;
#4323 = CLOSED_SHELL ( 'NONE', ( #5937, #3810, #3437, #5436, #4965, #5245, #3051, #3916, #4473, #1885, #5938, #4469, #6089, #2467, #5443, #3884, #693, #4823, #2111 ) ) ;
#4324 = MECHANICAL_DESIGN_GEOMETRIC_PRESENTATION_REPRESENTATION (  '', ( #4631 ), #739 ) ;
#4325 = DIRECTION ( 'NONE',  ( -0.000000000000000000, -0.000000000000000000, -1.000000000000000000 ) ) ;
#4326 = CARTESIAN_POINT ( 'NONE',  ( 0.000000000000000000, 0.000000000000000000, 48.00000000000000000 ) ) ;
#4327 = DIRECTION ( 'NONE',  ( 0.000000000000000000, 0.000000000000000000, 1.000000000000000000 ) ) ;
#4328 = VERTEX_POINT ( 'NONE', #2389 ) ;
#4329 = ORIENTED_EDGE ( 'NONE', *, *, #1260, .T. ) ;
#4330 = ORIENTED_EDGE ( 'NONE', *, *, #3453, .T. ) ;
#4331 = CARTESIAN_POINT ( 'NONE',  ( 0.000000000000000000, 120.0000000000000000, -4.000000000000000000 ) ) ;
#4332 = FACE_OUTER_BOUND ( 'NONE', #4055, .T. ) ;
#4333 = VECTOR ( 'NONE', #331, 1000.000000000000000 ) ;
#4334 = CARTESIAN_POINT ( 'NONE',  ( 10.99369682877389387, -22.46365890119677999, 6.219949983291193973 ) ) ;
#4335 = ORIENTED_EDGE ( 'NONE', *, *, #2662, .F. ) ;
#4336 = LINE ( 'NONE', #5314, #4585 ) ;
#4337 = DIRECTION ( 'NONE',  ( -0.000000000000000000, 0.000000000000000000, 1.000000000000000000 ) ) ;
#4338 = DIRECTION ( 'NONE',  ( -0.000000000000000000, -0.000000000000000000, 1.000000000000000000 ) ) ;
#4339 = CYLINDRICAL_SURFACE ( 'NONE', #5976, 22.67164836619068424 ) ;
#4340 = VERTEX_POINT ( 'NONE', #912 ) ;
#4341 = LINE ( 'NONE', #3802, #2551 ) ;
#4342 = CIRCLE ( 'NONE', #6002, 25.00000000000000000 ) ;
#4343 = FACE_OUTER_BOUND ( 'NONE', #459, .T. ) ;
#4344 = CARTESIAN_POINT ( 'NONE',  ( 0.000000000000000000, 0.000000000000000000, 44.00000000000000711 ) ) ;
#4345 = EDGE_CURVE ( 'NONE', #3440, #3708, #4921, .T. ) ;
#4346 = DIRECTION ( 'NONE',  ( -1.000000000000000000, 0.000000000000000000, 0.000000000000000000 ) ) ;
#4347 = CARTESIAN_POINT ( 'NONE',  ( 4.574218739510392595, -24.57872545437487588, 25.82634213602822726 ) ) ;
#4348 = VERTEX_POINT ( 'NONE', #799 ) ;
#4349 = DIRECTION ( 'NONE',  ( -1.000000000000000000, 0.000000000000000000, 0.000000000000000000 ) ) ;
#4350 = ORIENTED_EDGE ( 'NONE', *, *, #5698, .T. ) ;
#4351 = APPLICATION_CONTEXT ( 'automotive_design' ) ;
#4352 = CARTESIAN_POINT ( 'NONE',  ( -6.002163747819661666, 22.20348677930560655, 36.27767814654681899 ) ) ;
#4353 = EDGE_CURVE ( 'NONE', #427, #3554, #195, .T. ) ;
#4354 = DIRECTION ( 'NONE',  ( -0.000000000000000000, -0.000000000000000000, 1.000000000000000000 ) ) ;
#4355 = EDGE_CURVE ( 'NONE', #2452, #4562, #2135, .T. ) ;
#4356 = CARTESIAN_POINT ( 'NONE',  ( 44.64065620456912598, 28.99954194078667413, -110.0000000000000000 ) ) ;
#4357 = CARTESIAN_POINT ( 'NONE',  ( 132.0000000000000000, 69.00000000000000000, 110.0000000000000000 ) ) ;
#4358 = ORIENTED_EDGE ( 'NONE', *, *, #61, .T. ) ;
#4359 = ORIENTED_EDGE ( 'NONE', *, *, #1630, .T. ) ;
#4360 = EDGE_CURVE ( 'NONE', #5193, #1679, #5847, .T. ) ;
#4361 = EDGE_CURVE ( 'NONE', #3965, #1786, #2899, .T. ) ;
#4362 = EDGE_LOOP ( 'NONE', ( #5178, #1651, #474, #4185 ) ) ;
#4363 = CARTESIAN_POINT ( 'NONE',  ( 8.000000000000021316, 1.481987083124922376E-15, 12.00000000000000000 ) ) ;
#4364 = FACE_BOUND ( 'NONE', #1765, .T. ) ;
#4365 = CARTESIAN_POINT ( 'NONE',  ( 5.944036167333010212, -24.28654258472968408, 8.982995935198122339 ) ) ;
#4366 = ORIENTED_EDGE ( 'NONE', *, *, #1201, .T. ) ;
#4367 = PLANE ( 'NONE',  #3976 ) ;
#4368 = DIRECTION ( 'NONE',  ( 1.000000000000000000, 2.668814372793135769E-17, 1.269718898469700815E-21 ) ) ;
#4369 = CARTESIAN_POINT ( 'NONE',  ( -4.599867106623924506, -22.53795783706889821, 25.83444357079220666 ) ) ;
#4370 = DIRECTION ( 'NONE',  ( 1.000000000000000000, 0.000000000000000000, -0.000000000000000000 ) ) ;
#4371 = AXIS2_PLACEMENT_3D ( 'NONE', #5295, #943, #2895 ) ;
#4372 = CARTESIAN_POINT ( 'NONE',  ( -2.012341796004660122, 19.89850447888114005, 39.00000000000001421 ) ) ;
#4373 = EDGE_LOOP ( 'NONE', ( #2391, #4485, #4664, #319, #1824, #2863 ) ) ;
#4374 = AXIS2_PLACEMENT_3D ( 'NONE', #4031, #6076, #1653 ) ;
#4375 = FACE_BOUND ( 'NONE', #203, .T. ) ;
#4376 = PLANE ( 'NONE',  #5102 ) ;
#4377 = CARTESIAN_POINT ( 'NONE',  ( 1.953660101606555122, 24.92823101129173580, 24.51724137628377420 ) ) ;
#4378 = CARTESIAN_POINT ( 'NONE',  ( -13.40780655258107146, 26.42202358648259519, 5.467569244659289396 ) ) ;
#4379 = AXIS2_PLACEMENT_3D ( 'NONE', #4239, #1211, #4210 ) ;
#4380 = CARTESIAN_POINT ( 'NONE',  ( 0.000000000000000000, 0.000000000000000000, 12.00000000000000000 ) ) ;
#4381 = EDGE_LOOP ( 'NONE', ( #1909, #3582, #3070, #4771 ) ) ;
#4382 = EDGE_CURVE ( 'NONE', #5613, #2780, #5179, .T. ) ;
#4383 = CYLINDRICAL_SURFACE ( 'NONE', #1420, 25.00000000000000000 ) ;
#4384 = CARTESIAN_POINT ( 'NONE',  ( 13.27340567884428957, 26.93747317953756593, 8.027960515371223238 ) ) ;
#4385 = CARTESIAN_POINT ( 'NONE',  ( -3.081487911019577365E-30, 5.660601460262082306E-46, 281.0000000000000000 ) ) ;
#4386 = CIRCLE ( 'NONE', #4165, 24.99999999999999289 ) ;
#4387 = CARTESIAN_POINT ( 'NONE',  ( -2.546401178541497462E-16, -25.00000000000000000, 24.27501000028010125 ) ) ;
#4388 = AXIS2_PLACEMENT_3D ( 'NONE', #4408, #3892, #611 ) ;
#4389 = ADVANCED_FACE ( 'NONE', ( #433, #4718 ), #4383, .T. ) ;
#4390 = LINE ( 'NONE', #3971, #5228 ) ;
#4391 = FACE_OUTER_BOUND ( 'NONE', #5771, .T. ) ;
#4392 = ORIENTED_EDGE ( 'NONE', *, *, #5908, .T. ) ;
#4393 = ORIENTED_EDGE ( 'NONE', *, *, #189, .F. ) ;
#4394 = ORIENTED_EDGE ( 'NONE', *, *, #4883, .T. ) ;
#4395 = AXIS2_PLACEMENT_3D ( 'NONE', #6046, #6317, #3739 ) ;
#4396 = ORIENTED_EDGE ( 'NONE', *, *, #189, .T. ) ;
#4397 = EDGE_CURVE ( 'NONE', #1995, #768, #811, .T. ) ;
#4398 = DIRECTION ( 'NONE',  ( -0.000000000000000000, -0.000000000000000000, -1.000000000000000000 ) ) ;
#4399 = LINE ( 'NONE', #2465, #2144 ) ;
#4400 = EDGE_CURVE ( 'NONE', #3965, #2143, #3168, .T. ) ;
#4401 = AXIS2_PLACEMENT_3D ( 'NONE', #918, #1335, #1914 ) ;
#4402 = CARTESIAN_POINT ( 'NONE',  ( -11.89524262375575603, -21.99145298458226705, 5.444687415670875552 ) ) ;
#4403 = ORIENTED_EDGE ( 'NONE', *, *, #5169, .T. ) ;
#4404 = AXIS2_PLACEMENT_3D ( 'NONE', #5957, #928, #5407 ) ;
#4405 = ADVANCED_FACE ( 'NONE', ( #245, #2201 ), #4158, .F. ) ;
#4406 = DIRECTION ( 'NONE',  ( 1.000000000000000000, 0.000000000000000000, 0.000000000000000000 ) ) ;
#4407 = CARTESIAN_POINT ( 'NONE',  ( -23.00000000000000000, 0.000000000000000000, 39.00000000000001421 ) ) ;
#4408 = CARTESIAN_POINT ( 'NONE',  ( -8.000000000000003553, 100.3953136438507272, 5.999999999999999112 ) ) ;
#4409 = AXIS2_PLACEMENT_3D ( 'NONE', #3669, #3120, #5097 ) ;
#4410 = CARTESIAN_POINT ( 'NONE',  ( 0.000000000000000000, 0.000000000000000000, 39.00000000000001421 ) ) ;
#4411 = ORIENTED_EDGE ( 'NONE', *, *, #4637, .F. ) ;
#4412 = CARTESIAN_POINT ( 'NONE',  ( 0.6825543444542561122, 20.00000000000000000, 39.27501000028010480 ) ) ;
#4413 = EDGE_LOOP ( 'NONE', ( #5306, #4394 ) ) ;
#4414 = ADVANCED_FACE ( 'NONE', ( #561 ), #3546, .T. ) ;
#4415 = FACE_OUTER_BOUND ( 'NONE', #2779, .T. ) ;
#4416 = CIRCLE ( 'NONE', #1632, 20.00000000000000000 ) ;
#4417 = CARTESIAN_POINT ( 'NONE',  ( -13.27343467285272816, 26.93736435430921716, 3.972397629097670357 ) ) ;
#4418 = CIRCLE ( 'NONE', #2248, 12.50000000000001421 ) ;
#4419 = LINE ( 'NONE', #5481, #829 ) ;
#4420 = ORIENTED_EDGE ( 'NONE', *, *, #791, .T. ) ;
#4421 = DIRECTION ( 'NONE',  ( 0.000000000000000000, -1.740526192617802767E-17, -1.000000000000000000 ) ) ;
#4422 = B_SPLINE_CURVE_WITH_KNOTS ( 'NONE', 3,
 ( #6013, #3556, #3076, #5076, #4550, #3977, #1987, #4003, #5005, #1500, #666, #3952, #3586, #3465, #5438, #5987, #5042, #3498 ),
 .UNSPECIFIED., .F., .F.,
 ( 4, 2, 2, 2, 2, 2, 2, 2, 4 ),
 ( 0.006348828280262475490, 0.007141278029982640538, 0.007933727779702805585, 0.008726177529422970633, 0.009518627279143135680, 0.01031107702886330073, 0.01110352677858346578, 0.01189597652830363082, 0.01268842627802379587 ),
 .UNSPECIFIED. ) ;
#4423 = CARTESIAN_POINT ( 'NONE',  ( 13.19716647944431820, 27.23303957064661773, 8.463596398456379788 ) ) ;
#4424 = FACE_OUTER_BOUND ( 'NONE', #831, .T. ) ;
#4425 = AXIS2_PLACEMENT_3D ( 'NONE', #2612, #5068, #1191 ) ;
#4426 = DIRECTION ( 'NONE',  ( 1.000000000000000000, 0.000000000000000000, 0.000000000000000000 ) ) ;
#4427 = CARTESIAN_POINT ( 'NONE',  ( 132.0000000000000000, 69.00000000000000000, 110.0000000000000000 ) ) ;
#4428 = CARTESIAN_POINT ( 'NONE',  ( -17.00000000000000000, 25.00000000000000355, -30.00000000000000000 ) ) ;
#4429 = ORIENTED_EDGE ( 'NONE', *, *, #944, .T. ) ;
#4430 = AXIS2_PLACEMENT_3D ( 'NONE', #1481, #1055, #3893 ) ;
#4431 = ORIENTED_EDGE ( 'NONE', *, *, #5227, .F. ) ;
#4432 = VERTEX_POINT ( 'NONE', #1489 ) ;
#4433 = CIRCLE ( 'NONE', #4842, 22.00000000000000000 ) ;
#4434 = CARTESIAN_POINT ( 'NONE',  ( 17.00000000000000000, 0.000000000000000000, -273.0000000000000000 ) ) ;
#4435 = DIRECTION ( 'NONE',  ( -1.000000000000000000, 0.000000000000000000, -0.000000000000000000 ) ) ;
#4436 = CARTESIAN_POINT ( 'NONE',  ( 13.06023069425439864, -21.31967003585101850, 4.296371343529789222 ) ) ;
#4437 = ORIENTED_EDGE ( 'NONE', *, *, #2931, .T. ) ;
#4438 = MANIFOLD_SOLID_BREP ( 'Mirror10', #3190 ) ;
#4439 = AXIS2_PLACEMENT_3D ( 'NONE', #229, #3944, #3007 ) ;
#4440 = CARTESIAN_POINT ( 'NONE',  ( -6.137861079775116302, -22.16774101882030124, 27.44213700196646144 ) ) ;
#4441 = CARTESIAN_POINT ( 'NONE',  ( 0.000000000000000000, 0.000000000000000000, 12.00000000000000000 ) ) ;
#4442 = ORIENTED_EDGE ( 'NONE', *, *, #5347, .F. ) ;
#4443 = ORIENTED_EDGE ( 'NONE', *, *, #5263, .F. ) ;
#4444 = DIRECTION ( 'NONE',  ( -0.000000000000000000, -0.000000000000000000, -1.000000000000000000 ) ) ;
#4445 = FACE_OUTER_BOUND ( 'NONE', #1955, .T. ) ;
#4446 = CARTESIAN_POINT ( 'NONE',  ( 4.376116820636602789, 24.61487579939255355, 25.67915452354946737 ) ) ;
#4447 = CARTESIAN_POINT ( 'NONE',  ( 12.41746183822997551, 30.39531364385071299, 1.999999999999990008 ) ) ;
#4448 = CARTESIAN_POINT ( 'NONE',  ( 18.00000000000000355, 100.3953136438507272, 1.999999999999998224 ) ) ;
#4449 = EDGE_LOOP ( 'NONE', ( #3261, #6271 ) ) ;
#4450 = CARTESIAN_POINT ( 'NONE',  ( 25.00000000000000000, 3.061616997868383043E-15, 50.00000000000000711 ) ) ;
#4451 = VERTEX_POINT ( 'NONE', #2489 ) ;
#4452 = FACE_OUTER_BOUND ( 'NONE', #2939, .T. ) ;
#4453 = FACE_OUTER_BOUND ( 'NONE', #730, .T. ) ;
#4454 = VECTOR ( 'NONE', #663, 1000.000000000000000 ) ;
#4455 = CARTESIAN_POINT ( 'NONE',  ( 15.99408614349810698, 16.52843635781563592, 0.000000000000000000 ) ) ;
#4456 = CARTESIAN_POINT ( 'NONE',  ( 44.00000000000000000, -13.41640786499874771, -240.0000000000000000 ) ) ;
#4457 = ORIENTED_EDGE ( 'NONE', *, *, #6177, .F. ) ;
#4458 = ORIENTED_EDGE ( 'NONE', *, *, #5839, .F. ) ;
#4459 = ORIENTED_EDGE ( 'NONE', *, *, #4573, .T. ) ;
#4460 = DIRECTION ( 'NONE',  ( -0.000000000000000000, 0.000000000000000000, 1.000000000000000000 ) ) ;
#4461 = DIRECTION ( 'NONE',  ( 1.836970198721029194E-16, 1.000000000000000000, 0.000000000000000000 ) ) ;
#4462 = CARTESIAN_POINT ( 'NONE',  ( -8.933863590510668473, -23.35242969744760089, 7.599770008932984489 ) ) ;
#4463 = EDGE_LOOP ( 'NONE', ( #5675, #4535, #3820 ) ) ;
#4464 = DIRECTION ( 'NONE',  ( -0.000000000000000000, -0.000000000000000000, -1.000000000000000000 ) ) ;
#4465 = DIRECTION ( 'NONE',  ( -1.000000000000000000, 2.579192770663543253E-16, 3.976288500597762550E-16 ) ) ;
#4466 = CARTESIAN_POINT ( 'NONE',  ( -1.127325861074953917, -22.97343572093476638, 24.35677350376877470 ) ) ;
#4467 = DIRECTION ( 'NONE',  ( 0.000000000000000000, -1.000000000000000000, 0.000000000000000000 ) ) ;
#4468 = ORIENTED_EDGE ( 'NONE', *, *, #4580, .T. ) ;
#4469 = ADVANCED_FACE ( 'NONE', ( #1089 ), #5944, .F. ) ;
#4470 = CARTESIAN_POINT ( 'NONE',  ( 18.00000000000000355, 100.3953136438507272, 5.999999999999999112 ) ) ;
#4471 = CARTESIAN_POINT ( 'NONE',  ( 2.380270672502711906E-15, -5.204170427930421283E-15, -180.0000000000000000 ) ) ;
#4472 = DIRECTION ( 'NONE',  ( 1.000000000000000000, 0.000000000000000000, 0.000000000000000000 ) ) ;
#4473 = ADVANCED_FACE ( 'NONE', ( #73 ), #625, .T. ) ;
#4474 = ADVANCED_BREP_SHAPE_REPRESENTATION ( '', ( #151, #6349 ), #596 ) ;
#4475 = PLANE ( 'NONE',  #6172 ) ;
#4476 = ORIENTED_EDGE ( 'NONE', *, *, #801, .T. ) ;
#4477 = DIRECTION ( 'NONE',  ( 0.000000000000000000, 0.000000000000000000, 1.000000000000000000 ) ) ;
#4478 = AXIS2_PLACEMENT_3D ( 'NONE', #3090, #5058, #5506 ) ;
#4479 = CARTESIAN_POINT ( 'NONE',  ( -4.240260142090316542, 22.60916465144881826, 25.57229111368760854 ) ) ;
#4480 = EDGE_CURVE ( 'NONE', #1266, #1008, #3170, .T. ) ;
#4481 = LINE ( 'NONE', #5486, #4810 ) ;
#4482 = DIRECTION ( 'NONE',  ( -1.000000000000000000, 0.000000000000000000, 0.000000000000000000 ) ) ;
#4483 = EDGE_CURVE ( 'NONE', #624, #5536, #5973, .T. ) ;
#4484 = ORIENTED_EDGE ( 'NONE', *, *, #4361, .T. ) ;
#4485 = ORIENTED_EDGE ( 'NONE', *, *, #3541, .T. ) ;
#4486 = AXIS2_PLACEMENT_3D ( 'NONE', #4255, #3390, #1855 ) ;
#4487 = AXIS2_PLACEMENT_3D ( 'NONE', #2794, #5666, #1249 ) ;
#4488 = AXIS2_PLACEMENT_3D ( 'NONE', #1771, #3741, #3281 ) ;
#4489 = DIRECTION ( 'NONE',  ( -1.000000000000000000, 0.000000000000000000, 0.000000000000000000 ) ) ;
#4490 = DIRECTION ( 'NONE',  ( -0.000000000000000000, -0.000000000000000000, -1.000000000000000000 ) ) ;
#4491 = CIRCLE ( 'NONE', #2226, 166.8359700257217071 ) ;
#4492 = DIRECTION ( 'NONE',  ( 1.000000000000000000, 0.000000000000000000, -0.000000000000000000 ) ) ;
#4493 = ORIENTED_EDGE ( 'NONE', *, *, #5830, .T. ) ;
#4494 = AXIS2_PLACEMENT_3D ( 'NONE', #2742, #2296, #5720 ) ;
#4495 = APPLICATION_PROTOCOL_DEFINITION ( 'draft international standard', 'automotive_design', 1998, #4808 ) ;
#4496 = DIRECTION ( 'NONE',  ( 0.000000000000000000, 0.000000000000000000, 1.000000000000000000 ) ) ;
#4497 = DIRECTION ( 'NONE',  ( -0.000000000000000000, -0.000000000000000000, 1.000000000000000000 ) ) ;
#4498 = ORIENTED_EDGE ( 'NONE', *, *, #4480, .F. ) ;
#4499 = ORIENTED_EDGE ( 'NONE', *, *, #4833, .F. ) ;
#4500 = AXIS2_PLACEMENT_3D ( 'NONE', #1085, #2666, #101 ) ;
#4501 = DIRECTION ( 'NONE',  ( 0.000000000000000000, 0.000000000000000000, 1.000000000000000000 ) ) ;
#4502 = AXIS2_PLACEMENT_3D ( 'NONE', #3386, #6352, #1202 ) ;
#4503 = DIRECTION ( 'NONE',  ( 1.000000000000000000, 0.000000000000000000, 0.000000000000000000 ) ) ;
#4504 = CARTESIAN_POINT ( 'NONE',  ( 0.000000000000000000, -17.00000000000000000, 276.0000000000000000 ) ) ;
#4505 = EDGE_LOOP ( 'NONE', ( #2553, #4675, #2878, #568, #3567, #5708 ) ) ;
#4506 = SURFACE_STYLE_USAGE ( .BOTH. , #1009 ) ;
#4507 = VECTOR ( 'NONE', #364, 1000.000000000000000 ) ;
#4508 = LINE ( 'NONE', #109, #3917 ) ;
#4509 = CARTESIAN_POINT ( 'NONE',  ( -6.703346455576358665, 22.00175929117281015, 28.40382332099657958 ) ) ;
#4510 = VECTOR ( 'NONE', #5686, 1000.000000000000000 ) ;
#4511 = FACE_OUTER_BOUND ( 'NONE', #4738, .T. ) ;
#4512 = AXIS2_PLACEMENT_3D ( 'NONE', #1049, #4490, #5406 ) ;
#4513 = DIRECTION ( 'NONE',  ( -1.000000000000000000, 0.000000000000000000, 0.000000000000000000 ) ) ;
#4514 = EDGE_LOOP ( 'NONE', ( #1665, #782, #5163, #2375, #5340, #1960, #659, #898, #5943, #3717, #3849, #5113, #2814, #1851 ) ) ;
#4515 = VERTEX_POINT ( 'NONE', #4993 ) ;
#4516 = ORIENTED_EDGE ( 'NONE', *, *, #5270, .T. ) ;
#4517 = AXIS2_PLACEMENT_3D ( 'NONE', #6151, #2572, #750 ) ;
#4518 = DIRECTION ( 'NONE',  ( -0.000000000000000000, -0.000000000000000000, -1.000000000000000000 ) ) ;
#4519 = CARTESIAN_POINT ( 'NONE',  ( -44.64065620456893413, -28.99954194078699032, -30.00000000000000000 ) ) ;
#4520 = DIRECTION ( 'NONE',  ( 0.000000000000000000, 0.000000000000000000, 1.000000000000000000 ) ) ;
#4521 = CIRCLE ( 'NONE', #3505, 17.00000000000000000 ) ;
#4522 = LINE ( 'NONE', #935, #3153 ) ;
#4523 = FACE_OUTER_BOUND ( 'NONE', #192, .T. ) ;
#4524 = ORIENTED_EDGE ( 'NONE', *, *, #2354, .T. ) ;
#4525 = DIRECTION ( 'NONE',  ( -0.9999999999999998890, 1.376214178003270135E-17, 4.170629591192004883E-16 ) ) ;
#4526 = DIRECTION ( 'NONE',  ( 2.295390878742131754E-32, -1.239088197126290570E-16, 1.000000000000000000 ) ) ;
#4527 = VECTOR ( 'NONE', #5294, 1000.000000000000000 ) ;
#4528 = CIRCLE ( 'NONE', #122, 25.00000000000000000 ) ;
#4529 = PLANE ( 'NONE',  #4321 ) ;
#4530 = VERTEX_POINT ( 'NONE', #4450 ) ;
#4531 = DIRECTION ( 'NONE',  ( 1.000000000000000000, 0.000000000000000000, 0.000000000000000000 ) ) ;
#4532 = PLANE ( 'NONE',  #5520 ) ;
#4533 = AXIS2_PLACEMENT_3D ( 'NONE', #2889, #4337, #1028 ) ;
#4534 = FACE_BOUND ( 'NONE', #2147, .T. ) ;
#4535 = ORIENTED_EDGE ( 'NONE', *, *, #4546, .T. ) ;
#4536 = CARTESIAN_POINT ( 'NONE',  ( 10.40746208496127245, 20.52425257667962555, 6.660905398399123101 ) ) ;
#4537 = FILL_AREA_STYLE_COLOUR ( '', #941 ) ;
#4538 = CARTESIAN_POINT ( 'NONE',  ( -6.139315947428367615, 22.16738032098082911, 27.44370026704754650 ) ) ;
#4539 = CARTESIAN_POINT ( 'NONE',  ( -2.201053925086813301, 24.90665284231785392, 9.868642342566225523 ) ) ;
#4540 = CARTESIAN_POINT ( 'NONE',  ( 0.000000000000000000, 0.000000000000000000, -248.0000000000000000 ) ) ;
#4541 = VERTEX_POINT ( 'NONE', #3062 ) ;
#4542 = EDGE_LOOP ( 'NONE', ( #3876, #2626, #226, #3402 ) ) ;
#4543 = EDGE_LOOP ( 'NONE', ( #2399, #3623, #1037, #6342 ) ) ;
#4544 = EDGE_CURVE ( 'NONE', #5570, #1386, #150, .T. ) ;
#4545 = ORIENTED_EDGE ( 'NONE', *, *, #1600, .T. ) ;
#4546 = EDGE_CURVE ( 'NONE', #3869, #1294, #717, .T. ) ;
#4547 = CARTESIAN_POINT ( 'NONE',  ( 59.99991398172927859, 76.99999716619419132, 281.0000000000000000 ) ) ;
#4548 = AXIS2_PLACEMENT_3D ( 'NONE', #2362, #1464, #3006 ) ;
#4549 = EDGE_CURVE ( 'NONE', #3788, #2635, #2140, .T. ) ;
#4550 = CARTESIAN_POINT ( 'NONE',  ( 13.35991119780008418, 26.60492657425309559, 4.695075907386113911 ) ) ;
#4551 = DIRECTION ( 'NONE',  ( 1.000000000000000000, 0.000000000000000000, 0.000000000000000000 ) ) ;
#4552 = CYLINDRICAL_SURFACE ( 'NONE', #4804, 24.99999999999999289 ) ;
#4553 = EDGE_CURVE ( 'NONE', #4872, #1146, #3796, .T. ) ;
#4554 = EDGE_CURVE ( 'NONE', #6160, #1758, #6157, .T. ) ;
#4555 = CARTESIAN_POINT ( 'NONE',  ( -13.04517011400474580, -21.32889776003924709, 4.312637851115566967 ) ) ;
#4556 = VERTEX_POINT ( 'NONE', #172 ) ;
#4557 =( REPRESENTATION_RELATIONSHIP ('NONE','NONE', #632, #3711 ) REPRESENTATION_RELATIONSHIP_WITH_TRANSFORMATION ( #709 )SHAPE_REPRESENTATION_RELATIONSHIP( ) );
#4558 = DIRECTION ( 'NONE',  ( 1.298070219534905920E-15, 0.9868877816584453733, 0.1614078883241860107 ) ) ;
#4559 = CARTESIAN_POINT ( 'NONE',  ( -17.00000000000000000, 2.081899558550500280E-15, -248.0000000000000000 ) ) ;
#4560 = ORIENTED_EDGE ( 'NONE', *, *, #5427, .T. ) ;
#4561 = CARTESIAN_POINT ( 'NONE',  ( 279.0000000000000000, 0.000000000000000000, 0.000000000000000000 ) ) ;
#4562 = VERTEX_POINT ( 'NONE', #4141 ) ;
#4563 = ADVANCED_FACE ( 'NONE', ( #2697 ), #2125, .T. ) ;
#4564 = EDGE_CURVE ( 'NONE', #2487, #1781, #4702, .T. ) ;
#4565 = CARTESIAN_POINT ( 'NONE',  ( 0.000000000000000000, 0.000000000000000000, -4.000000000000000000 ) ) ;
#4566 = CARTESIAN_POINT ( 'NONE',  ( 0.000000000000000000, 120.0000000000000000, 16.00000000000000000 ) ) ;
#4567 = DIRECTION ( 'NONE',  ( -0.000000000000000000, 0.000000000000000000, -1.000000000000000000 ) ) ;
#4568 = CARTESIAN_POINT ( 'NONE',  ( 0.2052511266213299934, 21.25619793154162807, -195.0000000000000000 ) ) ;
#4569 = ORIENTED_EDGE ( 'NONE', *, *, #2077, .F. ) ;
#4570 = DIRECTION ( 'NONE',  ( 0.000000000000000000, 0.000000000000000000, 1.000000000000000000 ) ) ;
#4571 = CARTESIAN_POINT ( 'NONE',  ( -7.369598735940123824, 21.78745483514939707, 30.31133554494096671 ) ) ;
#4572 = CARTESIAN_POINT ( 'NONE',  ( -12.78450670028659530, 21.48642263404484964, 4.587769495204019776 ) ) ;
#4573 = EDGE_CURVE ( 'NONE', #3088, #4309, #204, .T. ) ;
#4574 = CARTESIAN_POINT ( 'NONE',  ( -44.43364355155666345, 29.42304313293565343, -65.00000000000000000 ) ) ;
#4575 = AXIS2_PLACEMENT_3D ( 'NONE', #6290, #1419, #3378 ) ;
#4576 = EDGE_LOOP ( 'NONE', ( #2285, #1917, #3615, #2669 ) ) ;
#4577 = AXIS2_PLACEMENT_3D ( 'NONE', #3085, #6052, #3594 ) ;
#4578 = ORIENTED_EDGE ( 'NONE', *, *, #4011, .F. ) ;
#4579 = DIRECTION ( 'NONE',  ( 0.000000000000000000, 0.000000000000000000, 1.000000000000000000 ) ) ;
#4580 = EDGE_CURVE ( 'NONE', #6130, #5682, #4822, .T. ) ;
#4581 = EDGE_CURVE ( 'NONE', #5659, #3152, #6268, .T. ) ;
#4582 = DIRECTION ( 'NONE',  ( -0.000000000000000000, -0.000000000000000000, -1.000000000000000000 ) ) ;
#4583 = CARTESIAN_POINT ( 'NONE',  ( -8.000000000000007105, 72.93807001241029297, 12.00000000000000000 ) ) ;
#4584 = DIRECTION ( 'NONE',  ( -0.000000000000000000, -0.000000000000000000, -1.000000000000000000 ) ) ;
#4585 = VECTOR ( 'NONE', #3404, 1000.000000000000000 ) ;
#4586 = DIRECTION ( 'NONE',  ( 0.000000000000000000, 0.000000000000000000, 1.000000000000000000 ) ) ;
#4587 = ORIENTED_EDGE ( 'NONE', *, *, #4124, .F. ) ;
#4588 = MANIFOLD_SOLID_BREP ( 'Fillet1', #838 ) ;
#4589 = EDGE_CURVE ( 'NONE', #5800, #2301, #1317, .T. ) ;
#4590 = ADVANCED_FACE ( 'NONE', ( #4665 ), #4218, .T. ) ;
#4591 = DIRECTION ( 'NONE',  ( -0.000000000000000000, -0.000000000000000000, -1.000000000000000000 ) ) ;
#4592 = AXIS2_PLACEMENT_3D ( 'NONE', #5046, #2917, #2411 ) ;
#4593 = ORIENTED_EDGE ( 'NONE', *, *, #5559, .T. ) ;
#4594 = FACE_OUTER_BOUND ( 'NONE', #490, .T. ) ;
#4595 = ORIENTED_EDGE ( 'NONE', *, *, #4756, .T. ) ;
#4596 = ADVANCED_FACE ( 'NONE', ( #1417 ), #5359, .F. ) ;
#4597 = DIRECTION ( 'NONE',  ( -1.000000000000000000, 0.000000000000000000, 0.000000000000000000 ) ) ;
#4598 = PLANE ( 'NONE',  #2894 ) ;
#4599 = DIRECTION ( 'NONE',  ( 0.000000000000000000, 0.000000000000000000, 1.000000000000000000 ) ) ;
#4600 = CIRCLE ( 'NONE', #188, 21.00000000000000355 ) ;
#4601 = DIRECTION ( 'NONE',  ( -1.000000000000000000, 0.000000000000000000, 0.000000000000000000 ) ) ;
#4602 = VERTEX_POINT ( 'NONE', #3775 ) ;
#4603 = EDGE_CURVE ( 'NONE', #53, #5357, #1844, .T. ) ;
#4604 = CARTESIAN_POINT ( 'NONE',  ( 0.000000000000000000, 76.99999716619419132, 0.000000000000000000 ) ) ;
#4605 = CARTESIAN_POINT ( 'NONE',  ( 174.7835321302054865, 68.75545066608756883, 1.999999999999994893 ) ) ;
#4606 = CARTESIAN_POINT ( 'NONE',  ( 5.735021534702854140, 22.27575375288411408, 36.62858606677772144 ) ) ;
#4607 = VECTOR ( 'NONE', #3106, 1000.000000000000000 ) ;
#4608 = CARTESIAN_POINT ( 'NONE',  ( 0.000000000000000000, 0.000000000000000000, 0.000000000000000000 ) ) ;
#4609 = MANIFOLD_SOLID_BREP ( 'Mirror2', #4323 ) ;
#4610 = CARTESIAN_POINT ( 'NONE',  ( -16.23652742703189489, -37.28747423195188304, -130.0000000000000000 ) ) ;
#4611 = ORIENTED_EDGE ( 'NONE', *, *, #6219, .F. ) ;
#4612 = PRESENTATION_LAYER_ASSIGNMENT (  '', '', ( #6060 ) ) ;
#4613 = VERTEX_POINT ( 'NONE', #4278 ) ;
#4614 = ORIENTED_EDGE ( 'NONE', *, *, #5795, .F. ) ;
#4615 = DIRECTION ( 'NONE',  ( 1.000000000000000000, 0.000000000000000000, 0.000000000000000000 ) ) ;
#4616 = AXIS2_PLACEMENT_3D ( 'NONE', #3499, #4917, #4004 ) ;
#4617 = PRODUCT_DEFINITION_SHAPE ( 'NONE', 'NONE',  #6371 ) ;
#4618 = CYLINDRICAL_SURFACE ( 'NONE', #1084, 22.67164836619067714 ) ;
#4619 = DIRECTION ( 'NONE',  ( 0.000000000000000000, 0.000000000000000000, 1.000000000000000000 ) ) ;
#4620 = CARTESIAN_POINT ( 'NONE',  ( 0.000000000000000000, 25.00000000000000000, -7.790539539321167162 ) ) ;
#4621 = CIRCLE ( 'NONE', #5549, 89.87058297576892585 ) ;
#4622 = CYLINDRICAL_SURFACE ( 'NONE', #5854, 19.00000000000000000 ) ;
#4623 = EDGE_LOOP ( 'NONE', ( #2460, #5329, #4105, #2567 ) ) ;
#4624 = CARTESIAN_POINT ( 'NONE',  ( -2.385244779468109755E-15, -1.040834085586084257E-14, -110.0000000000000000 ) ) ;
#4625 = CIRCLE ( 'NONE', #1641, 90.00000000000319744 ) ;
#4626 = CARTESIAN_POINT ( 'NONE',  ( -6.011784583892834100, -22.20189362571451142, 36.28151155367954317 ) ) ;
#4627 = VERTEX_POINT ( 'NONE', #5780 ) ;
#4628 = DIRECTION ( 'NONE',  ( 1.000000000000000000, 0.000000000000000000, 0.000000000000000000 ) ) ;
#4629 = VERTEX_POINT ( 'NONE', #2760 ) ;
#4630 = CARTESIAN_POINT ( 'NONE',  ( -19.00000000000000000, 0.000000000000000000, 15.00000000000000000 ) ) ;
#4631=STYLED_ITEM('',(#6419),#365);
#4632 = FACE_OUTER_BOUND ( 'NONE', #2886, .T. ) ;
#4633 = DIRECTION ( 'NONE',  ( 1.000000000000000000, 0.000000000000000000, 0.000000000000000000 ) ) ;
#4634 = DIRECTION ( 'NONE',  ( 0.000000000000000000, 0.000000000000000000, -1.000000000000000000 ) ) ;
#4635 = VERTEX_POINT ( 'NONE', #1381 ) ;
#4636 = EDGE_CURVE ( 'NONE', #5193, #3828, #818, .T. ) ;
#4637 = EDGE_CURVE ( 'NONE', #1077, #5724, #2352, .T. ) ;
#4638 = CARTESIAN_POINT ( 'NONE',  ( 265.0000000000000000, 14.00000000000000000, 0.000000000000000000 ) ) ;
#4639 = DIRECTION ( 'NONE',  ( -1.000000000000000000, 0.000000000000000000, 0.000000000000000000 ) ) ;
#4640 = DIRECTION ( 'NONE',  ( -0.000000000000000000, -0.000000000000000000, -1.000000000000000000 ) ) ;
#4641 = CIRCLE ( 'NONE', #5473, 17.00000000000000000 ) ;
#4642 = CARTESIAN_POINT ( 'NONE',  ( 15.22537606545850508, 19.83673216789829752, 1.447296480073241076 ) ) ;
#4643 = CARTESIAN_POINT ( 'NONE',  ( 13.14183123006952947, -39.58265509608667543, -65.00000000000000000 ) ) ;
#4644 = ORIENTED_EDGE ( 'NONE', *, *, #700, .T. ) ;
#4645 = VERTEX_POINT ( 'NONE', #3284 ) ;
#4646 = CARTESIAN_POINT ( 'NONE',  ( 44.64065620456912598, 28.99954194078667413, -95.00000000000000000 ) ) ;
#4647 = DIRECTION ( 'NONE',  ( -0.000000000000000000, -0.000000000000000000, -1.000000000000000000 ) ) ;
#4648 = DIRECTION ( 'NONE',  ( -0.000000000000000000, -0.000000000000000000, -1.000000000000000000 ) ) ;
#4649 = DIRECTION ( 'NONE',  ( -0.000000000000000000, -0.000000000000000000, -1.000000000000000000 ) ) ;
#4650 = DIRECTION ( 'NONE',  ( -0.000000000000000000, -0.000000000000000000, -1.000000000000000000 ) ) ;
#4651 = EDGE_LOOP ( 'NONE', ( #4016, #3476, #1543, #6337 ) ) ;
#4652 = DIRECTION ( 'NONE',  ( 1.000000000000000000, 0.000000000000000000, 0.000000000000000000 ) ) ;
#4653 = APPLICATION_PROTOCOL_DEFINITION ( 'draft international standard', 'automotive_design', 1998, #167 ) ;
#4654 = DIRECTION ( 'NONE',  ( -0.000000000000000000, -0.000000000000000000, -1.000000000000000000 ) ) ;
#4655 = ORIENTED_EDGE ( 'NONE', *, *, #2973, .F. ) ;
#4656 = EDGE_CURVE ( 'NONE', #4195, #4556, #6226, .T. ) ;
#4657 = CARTESIAN_POINT ( 'NONE',  ( 0.000000000000000000, 0.000000000000000000, -273.0000000000000000 ) ) ;
#4658 = ORIENTED_EDGE ( 'NONE', *, *, #4879, .T. ) ;
#4659 = DIRECTION ( 'NONE',  ( -0.000000000000000000, -0.000000000000000000, -1.000000000000000000 ) ) ;
#4660 = EDGE_CURVE ( 'NONE', #5958, #221, #4086, .T. ) ;
#4661 = DIRECTION ( 'NONE',  ( -0.000000000000000000, -0.000000000000000000, 1.000000000000000000 ) ) ;
#4662 = DIRECTION ( 'NONE',  ( -1.000000000000000000, 0.000000000000000000, 0.000000000000000000 ) ) ;
#4663 = FACE_OUTER_BOUND ( 'NONE', #512, .T. ) ;
#4664 = ORIENTED_EDGE ( 'NONE', *, *, #4670, .T. ) ;
#4665 = FACE_OUTER_BOUND ( 'NONE', #652, .T. ) ;
#4666 = VERTEX_POINT ( 'NONE', #1841 ) ;
#4667 = PRODUCT ( 'Part 32,2_Varsay\X2\0131\X0\lan', 'Part 32,2_Varsay\X2\0131\X0\lan', '', ( #1565 ) ) ;
#4668 = CARTESIAN_POINT ( 'NONE',  ( 0.000000000000000000, 69.00000000000000000, 0.000000000000000000 ) ) ;
#4669 = LINE ( 'NONE', #6195, #654 ) ;
#4670 = EDGE_CURVE ( 'NONE', #221, #2750, #4341, .T. ) ;
#4671 = EDGE_CURVE ( 'NONE', #2780, #3220, #2556, .T. ) ;
#4672 = CARTESIAN_POINT ( 'NONE',  ( -13.85467998626346819, 20.81921389911402542, 3.398299129130501139 ) ) ;
#4673 = FACE_OUTER_BOUND ( 'NONE', #6216, .T. ) ;
#4674 = VERTEX_POINT ( 'NONE', #972 ) ;
#4675 = ORIENTED_EDGE ( 'NONE', *, *, #3736, .F. ) ;
#4676 = ADVANCED_FACE ( 'NONE', ( #1968 ), #3934, .T. ) ;
#4677 = CARTESIAN_POINT ( 'NONE',  ( -5.648970382492173314, 24.35596037157667126, 26.81763994746973623 ) ) ;
#4678 = FACE_OUTER_BOUND ( 'NONE', #4463, .T. ) ;
#4679 = EDGE_CURVE ( 'NONE', #6010, #2034, #1426, .T. ) ;
#4680 = CARTESIAN_POINT ( 'NONE',  ( 44.56092774862622719, -29.44644455561813956, 0.000000000000000000 ) ) ;
#4681 = CARTESIAN_POINT ( 'NONE',  ( 0.000000000000000000, 25.00000000000000000, 301.0000000000000568 ) ) ;
#4682 = EDGE_CURVE ( 'NONE', #5198, #2238, #2239, .T. ) ;
#4683 = CIRCLE ( 'NONE', #263, 166.8359700257217071 ) ;
#4684 = ORIENTED_EDGE ( 'NONE', *, *, #3017, .T. ) ;
#4685 = DIRECTION ( 'NONE',  ( -1.000000000000000000, -1.852483853906148286E-16, 0.000000000000000000 ) ) ;
#4686 = ORIENTED_EDGE ( 'NONE', *, *, #1996, .F. ) ;
#4687 = EDGE_CURVE ( 'NONE', #2247, #1460, #3365, .T. ) ;
#4688 = SURFACE_STYLE_USAGE ( .BOTH. , #740 ) ;
#4689 = CARTESIAN_POINT ( 'NONE',  ( 8.997257985596670338, -21.18070524412206623, 7.578991052498396996 ) ) ;
#4690 = ORIENTED_EDGE ( 'NONE', *, *, #3467, .F. ) ;
#4691 = CARTESIAN_POINT ( 'NONE',  ( 19.25293315802950644, 8.385974291186926166, 12.00000000000000000 ) ) ;
#4692 = ORIENTED_EDGE ( 'NONE', *, *, #4603, .T. ) ;
#4693 = VECTOR ( 'NONE', #3164, 1000.000000000000000 ) ;
#4694 = DIRECTION ( 'NONE',  ( 0.000000000000000000, 0.000000000000000000, -1.000000000000000000 ) ) ;
#4695 = VECTOR ( 'NONE', #2605, 1000.000000000000000 ) ;
#4696 = PRODUCT_DEFINITION_CONTEXT ( 'detailed design', #3361, 'design' ) ;
#4697 = CARTESIAN_POINT ( 'NONE',  ( 0.000000000000000000, 120.0000000000000000, 12.00000000000000000 ) ) ;
#4698 = CARTESIAN_POINT ( 'NONE',  ( -8.000000000000021316, 1.729804722550182166E-15, 9.999999999999987566 ) ) ;
#4699 = DIRECTION ( 'NONE',  ( -1.000000000000000000, 0.000000000000000000, 0.000000000000000000 ) ) ;
#4700 = EDGE_LOOP ( 'NONE', ( #5152, #4007, #1087, #921 ) ) ;
#4701 = AXIS2_PLACEMENT_3D ( 'NONE', #3374, #2378, #425 ) ;
#4702 = LINE ( 'NONE', #4604, #411 ) ;
#4703 = VERTEX_POINT ( 'NONE', #1483 ) ;
#4704 = CARTESIAN_POINT ( 'NONE',  ( 7.307255365082232501, 23.90829471491150571, 30.06775954199970258 ) ) ;
#4705 = CYLINDRICAL_SURFACE ( 'NONE', #3766, 89.87058297576894006 ) ;
#4706 = CIRCLE ( 'NONE', #2844, 17.00000000000000000 ) ;
#4707 = CARTESIAN_POINT ( 'NONE',  ( -15.82602517378898987, 37.28747423195201094, 15.00000000000000000 ) ) ;
#4708 = CARTESIAN_POINT ( 'NONE',  ( 0.9883880857196321035, -24.98510658176930832, 24.32423833034778582 ) ) ;
#4709 = ORIENTED_EDGE ( 'NONE', *, *, #4549, .F. ) ;
#4710 = VECTOR ( 'NONE', #3726, 1000.000000000000000 ) ;
#4711 = ORIENTED_EDGE ( 'NONE', *, *, #249, .F. ) ;
#4712 = LINE ( 'NONE', #4151, #1371 ) ;
#4713 = DIRECTION ( 'NONE',  ( 1.000000000000000000, 0.000000000000000000, 0.000000000000000000 ) ) ;
#4714 = DIRECTION ( 'NONE',  ( 0.000000000000000000, 0.000000000000000000, 1.000000000000000000 ) ) ;
#4715 = CIRCLE ( 'NONE', #2051, 22.67164836619067714 ) ;
#4716 = CARTESIAN_POINT ( 'NONE',  ( 22.21770253897382474, 3.871672004622519037, -115.0000000000000000 ) ) ;
#4717 = EDGE_LOOP ( 'NONE', ( #1018, #20 ) ) ;
#4718 = FACE_BOUND ( 'NONE', #5974, .T. ) ;
#4719 = ORIENTED_EDGE ( 'NONE', *, *, #4000, .F. ) ;
#4720 = AXIS2_PLACEMENT_3D ( 'NONE', #2590, #3133, #4551 ) ;
#4721 = CARTESIAN_POINT ( 'NONE',  ( 2.380270672502711906E-15, -5.204170427930421283E-15, -45.00000000000000000 ) ) ;
#4722 = APPLICATION_PROTOCOL_DEFINITION ( 'draft international standard', 'automotive_design', 1998, #3699 ) ;
#4723 = CARTESIAN_POINT ( 'NONE',  ( 0.000000000000000000, 0.000000000000000000, 48.00000000000000000 ) ) ;
#4724 = AXIS2_PLACEMENT_3D ( 'NONE', #6303, #4327, #5761 ) ;
#4725 = EDGE_LOOP ( 'NONE', ( #3356, #5578, #3202, #1340 ) ) ;
#4726 = AXIS2_PLACEMENT_3D ( 'NONE', #4230, #1430, #888 ) ;
#4727 = VECTOR ( 'NONE', #1763, 1000.000000000000000 ) ;
#4728 = FACE_OUTER_BOUND ( 'NONE', #5305, .T. ) ;
#4729 = ORIENTED_EDGE ( 'NONE', *, *, #2982, .T. ) ;
#4730 = CIRCLE ( 'NONE', #3289, 90.00000000000319744 ) ;
#4731 = CARTESIAN_POINT ( 'NONE',  ( 0.000000000000000000, 76.99999716619419132, 0.000000000000000000 ) ) ;
#4732 = DIRECTION ( 'NONE',  ( -0.000000000000000000, 0.000000000000000000, -1.000000000000000000 ) ) ;
#4733 = DIRECTION ( 'NONE',  ( 0.000000000000000000, 1.000000000000000000, 1.740526192617802767E-17 ) ) ;
#4734 = AXIS2_PLACEMENT_3D ( 'NONE', #4133, #1568, #3177 ) ;
#4735 = CARTESIAN_POINT ( 'NONE',  ( -7.401918722292613495, -23.87915698552384569, 33.00856600121881712 ) ) ;
#4736 = ORIENTED_EDGE ( 'NONE', *, *, #1122, .T. ) ;
#4737 =( NAMED_UNIT ( * ) SI_UNIT ( $, .STERADIAN. ) SOLID_ANGLE_UNIT ( ) );
#4738 = EDGE_LOOP ( 'NONE', ( #5554, #6225, #4238, #798 ) ) ;
#4739 = CARTESIAN_POINT ( 'NONE',  ( 5.952041157299182039, 24.28165242506072374, 36.34480154750762182 ) ) ;
#4740 = CARTESIAN_POINT ( 'NONE',  ( 44.00000000000009948, 13.41640786499835514, -110.0000000000000000 ) ) ;
#4741 = CARTESIAN_POINT ( 'NONE',  ( 0.000000000000000000, 0.000000000000000000, 15.00000000000000000 ) ) ;
#4742 = AXIS2_PLACEMENT_3D ( 'NONE', #557, #2922, #4899 ) ;
#4743 = AXIS2_PLACEMENT_3D ( 'NONE', #4331, #2842, #4818 ) ;
#4744 = CARTESIAN_POINT ( 'NONE',  ( 7.451526880251365448, -23.86388513668106270, 30.79056676978083829 ) ) ;
#4745 = ORIENTED_EDGE ( 'NONE', *, *, #4768, .T. ) ;
#4746 = EDGE_LOOP ( 'NONE', ( #2900, #5585 ) ) ;
#4747 = CARTESIAN_POINT ( 'NONE',  ( -5.640759563529088361, 24.35584729907772683, 36.72391480687586807 ) ) ;
#4748 = DIRECTION ( 'NONE',  ( -0.000000000000000000, -0.000000000000000000, -1.000000000000000000 ) ) ;
#4749 = LINE ( 'NONE', #2396, #5953 ) ;
#4750 = LINE ( 'NONE', #3298, #5249 ) ;
#4751 = EDGE_CURVE ( 'NONE', #2498, #3061, #3069, .T. ) ;
#4752 = EDGE_LOOP ( 'NONE', ( #349, #2224 ) ) ;
#4753 = ADVANCED_FACE ( 'NONE', ( #6344 ), #2996, .F. ) ;
#4754 = VERTEX_POINT ( 'NONE', #2414 ) ;
#4755 = ORIENTED_EDGE ( 'NONE', *, *, #4058, .T. ) ;
#4756 = EDGE_CURVE ( 'NONE', #5184, #4635, #4715, .T. ) ;
#4757 = SURFACE_STYLE_FILL_AREA ( #1303 ) ;
#4758 = EDGE_CURVE ( 'NONE', #823, #81, #2960, .T. ) ;
#4759 = ADVANCED_FACE ( 'NONE', ( #1998 ), #520, .T. ) ;
#4760 = CARTESIAN_POINT ( 'NONE',  ( 0.000000000000000000, 0.000000000000000000, 47.00000000000000000 ) ) ;
#4761 = FACE_OUTER_BOUND ( 'NONE', #5081, .T. ) ;
#4762 = ORIENTED_EDGE ( 'NONE', *, *, #327, .T. ) ;
#4763 = CARTESIAN_POINT ( 'NONE',  ( 0.000000000000000000, 0.000000000000000000, 44.00000000000000711 ) ) ;
#4764 = ORIENTED_EDGE ( 'NONE', *, *, #5167, .F. ) ;
#4765 = CARTESIAN_POINT ( 'NONE',  ( -16.23652742703189489, -37.28747423195188304, -110.0000000000000000 ) ) ;
#4766 = TOROIDAL_SURFACE ( 'NONE', #1154, 6.500000000000000000, 1.000000000000000000 ) ;
#4767 = DIRECTION ( 'NONE',  ( 0.000000000000000000, 0.000000000000000000, -1.000000000000000000 ) ) ;
#4768 = EDGE_CURVE ( 'NONE', #1997, #5753, #4897, .T. ) ;
#4769 = FACE_BOUND ( 'NONE', #3178, .T. ) ;
#4770 = CARTESIAN_POINT ( 'NONE',  ( -0.2052511266214760433, -21.25619793154163517, -130.0000000000000000 ) ) ;
#4771 = ORIENTED_EDGE ( 'NONE', *, *, #6189, .F. ) ;
#4772 = CARTESIAN_POINT ( 'NONE',  ( -2.012341796004660122, 19.89850447888114005, 39.00000000000001421 ) ) ;
#4773 = LINE ( 'NONE', #5677, #5390 ) ;
#4774 = CARTESIAN_POINT ( 'NONE',  ( 17.00000000000000000, 69.00000000000000000, 0.000000000000000000 ) ) ;
#4775 = CARTESIAN_POINT ( 'NONE',  ( 6.737430854173819483, -24.07581932788624357, 28.44406090190429737 ) ) ;
#4776 = EDGE_LOOP ( 'NONE', ( #2325, #5952, #4392, #5725 ) ) ;
#4777 = ORIENTED_EDGE ( 'NONE', *, *, #5270, .F. ) ;
#4778 = CARTESIAN_POINT ( 'NONE',  ( -7.245258220727285980, 23.92722011157075812, 29.82133114287520925 ) ) ;
#4779 = ADVANCED_FACE ( 'NONE', ( #4375, #1935 ), #2028, .F. ) ;
#4780 = DIRECTION ( 'NONE',  ( -1.000000000000000000, 0.000000000000000000, 0.000000000000000000 ) ) ;
#4781 = DIRECTION ( 'NONE',  ( 0.000000000000000000, -1.000000000000000000, 1.740526192617802767E-17 ) ) ;
#4782 = CARTESIAN_POINT ( 'NONE',  ( 22.21770253897382474, 3.871672004622519037, -65.00000000000000000 ) ) ;
#4783 = VERTEX_POINT ( 'NONE', #3022 ) ;
#4784 = EDGE_LOOP ( 'NONE', ( #1472, #5442 ) ) ;
#4785 = CARTESIAN_POINT ( 'NONE',  ( -6.500000000000000000, 134.5953136438507158, 12.00000000000000000 ) ) ;
#4786 = DIRECTION ( 'NONE',  ( -0.000000000000000000, -0.000000000000000000, -1.000000000000000000 ) ) ;
#4787 = CARTESIAN_POINT ( 'NONE',  ( 16.99999999999999645, -25.00000000000000000, -65.00000000000000000 ) ) ;
#4788 = EDGE_LOOP ( 'NONE', ( #3269, #1581, #2164, #4227 ) ) ;
#4789 = ADVANCED_FACE ( 'NONE', ( #583, #3895 ), #5875, .T. ) ;
#4790 = AXIS2_PLACEMENT_3D ( 'NONE', #1938, #3896, #1999 ) ;
#4791 = AXIS2_PLACEMENT_3D ( 'NONE', #2438, #3436, #1 ) ;
#4792 = DIRECTION ( 'NONE',  ( 1.000000000000000000, 3.576835832488757469E-15, 0.000000000000000000 ) ) ;
#4793 =( NAMED_UNIT ( * ) SI_UNIT ( $, .STERADIAN. ) SOLID_ANGLE_UNIT ( ) );
#4794 = CARTESIAN_POINT ( 'NONE',  ( 17.05141243254541550, -24.25762350764758679, 0.000000000000000000 ) ) ;
#4795 = PLANE ( 'NONE',  #3661 ) ;
#4796 = DIRECTION ( 'NONE',  ( 1.000000000000000000, 0.000000000000000000, 0.000000000000000000 ) ) ;
#4797 = EDGE_LOOP ( 'NONE', ( #5836, #1954, #2652, #6193 ) ) ;
#4798 = CIRCLE ( 'NONE', #4276, 89.87058297576892585 ) ;
#4799 = CIRCLE ( 'NONE', #5624, 17.00000000000000000 ) ;
#4801 = CARTESIAN_POINT ( 'NONE',  ( 7.257437786822880099, 23.92362332953075565, 33.72945147699581980 ) ) ;
#4800 = CIRCLE ( 'NONE', #3887, 46.00000000000000000 ) ;
#4802 = DIRECTION ( 'NONE',  ( 0.000000000000000000, 0.000000000000000000, 1.000000000000000000 ) ) ;
#4803 = DIRECTION ( 'NONE',  ( 1.000000000000000000, 0.000000000000000000, 0.000000000000000000 ) ) ;
#4804 = AXIS2_PLACEMENT_3D ( 'NONE', #4060, #3929, #154 ) ;
#4805 = CARTESIAN_POINT ( 'NONE',  ( 7.500225230914490560, -23.84840920358612948, 32.26396939133217501 ) ) ;
#4806 = ORIENTED_EDGE ( 'NONE', *, *, #3257, .F. ) ;
#4807 = ORIENTED_EDGE ( 'NONE', *, *, #699, .F. ) ;
#4808 = APPLICATION_CONTEXT ( 'automotive_design' ) ;
#4809 = CARTESIAN_POINT ( 'NONE',  ( 0.000000000000000000, 0.000000000000000000, 1.000000000000000888 ) ) ;
#4810 = VECTOR ( 'NONE', #3034, 1000.000000000000000 ) ;
#4811 = DIRECTION ( 'NONE',  ( -1.000000000000000000, 0.000000000000000000, 0.000000000000000000 ) ) ;
#4812 = FACE_OUTER_BOUND ( 'NONE', #3819, .T. ) ;
#4813 = DIRECTION ( 'NONE',  ( 0.000000000000000000, 0.000000000000000000, -1.000000000000000000 ) ) ;
#4814 = AXIS2_PLACEMENT_3D ( 'NONE', #1515, #948, #4472 ) ;
#4815 = VERTEX_POINT ( 'NONE', #3304 ) ;
#4816 = ORIENTED_EDGE ( 'NONE', *, *, #2973, .T. ) ;
#4817 = CIRCLE ( 'NONE', #3790, 1.000000000000000000 ) ;
#4818 = DIRECTION ( 'NONE',  ( 1.000000000000000000, 0.000000000000000000, 0.000000000000000000 ) ) ;
#4819 = LINE ( 'NONE', #3762, #4090 ) ;
#4820 = CARTESIAN_POINT ( 'NONE',  ( 0.4617977782627283867, -24.99947972102657801, 9.999268903951906040 ) ) ;
#4821 = ORIENTED_EDGE ( 'NONE', *, *, #607, .F. ) ;
#4822 = CIRCLE ( 'NONE', #5650, 25.00000000000000000 ) ;
#4823 = ADVANCED_FACE ( 'NONE', ( #4761 ), #1793, .T. ) ;
#4824 = DIRECTION ( 'NONE',  ( -0.000000000000000000, -0.000000000000000000, -1.000000000000000000 ) ) ;
#4825 = AXIS2_PLACEMENT_3D ( 'NONE', #920, #2426, #3392 ) ;
#4826 = CARTESIAN_POINT ( 'NONE',  ( -17.00000000000000000, 2.081899558550500280E-15, -49.99999999999999289 ) ) ;
#4827 = VECTOR ( 'NONE', #5590, 1000.000000000000000 ) ;
#4828 = CIRCLE ( 'NONE', #5656, 45.99999999999997868 ) ;
#4829 = DIRECTION ( 'NONE',  ( -0.000000000000000000, -0.000000000000000000, -1.000000000000000000 ) ) ;
#4830 = DIRECTION ( 'NONE',  ( -1.000000000000000000, 0.000000000000000000, 0.000000000000000000 ) ) ;
#4831 = VERTEX_POINT ( 'NONE', #2843 ) ;
#4832 = AXIS2_PLACEMENT_3D ( 'NONE', #3543, #977, #4868 ) ;
#4833 = EDGE_CURVE ( 'NONE', #5651, #5709, #4819, .T. ) ;
#4834 = CYLINDRICAL_SURFACE ( 'NONE', #2211, 17.00000000000000000 ) ;
#4835 = ADVANCED_FACE ( 'NONE', ( #895 ), #4299, .T. ) ;
#4836 = AXIS2_PLACEMENT_3D ( 'NONE', #4657, #1597, #5535 ) ;
#4837 = EDGE_CURVE ( 'NONE', #4, #2027, #6277, .T. ) ;
#4838 = ADVANCED_FACE ( 'NONE', ( #4332 ), #1373, .F. ) ;
#4839 = CARTESIAN_POINT ( 'NONE',  ( 0.000000000000000000, 0.000000000000000000, 0.000000000000000000 ) ) ;
#4840 = CARTESIAN_POINT ( 'NONE',  ( 0.8980764441730644254, -22.98681745009828248, 24.31513574047610504 ) ) ;
#4841 = ORIENTED_EDGE ( 'NONE', *, *, #2469, .F. ) ;
#4842 = AXIS2_PLACEMENT_3D ( 'NONE', #562, #4477, #2545 ) ;
#4843 = DIRECTION ( 'NONE',  ( 1.000000000000000000, 0.000000000000000000, 0.000000000000000000 ) ) ;
#4844 = VERTEX_POINT ( 'NONE', #6310 ) ;
#4845 = AXIS2_PLACEMENT_3D ( 'NONE', #6142, #5664, #1245 ) ;
#4846 = LINE ( 'NONE', #1980, #1263 ) ;
#4847 = DIRECTION ( 'NONE',  ( 1.000000000000000000, 0.000000000000000000, -0.000000000000000000 ) ) ;
#4848 = CARTESIAN_POINT ( 'NONE',  ( 0.000000000000000000, 0.000000000000000000, -45.00000000000000000 ) ) ;
#4849 = DIRECTION ( 'NONE',  ( -1.000000000000000000, 0.000000000000000000, 0.000000000000000000 ) ) ;
#4850 = ORIENTED_EDGE ( 'NONE', *, *, #3129, .T. ) ;
#4851 = ORIENTED_EDGE ( 'NONE', *, *, #4656, .T. ) ;
#4852 = FACE_OUTER_BOUND ( 'NONE', #5665, .T. ) ;
#4853 = DIRECTION ( 'NONE',  ( 0.000000000000000000, 0.000000000000000000, -1.000000000000000000 ) ) ;
#4854 = AXIS2_PLACEMENT_3D ( 'NONE', #2344, #1802, #3798 ) ;
#4855 = ORIENTED_EDGE ( 'NONE', *, *, #2081, .F. ) ;
#4856 = DIRECTION ( 'NONE',  ( 1.000000000000000000, 0.000000000000000000, 0.000000000000000000 ) ) ;
#4857 = CARTESIAN_POINT ( 'NONE',  ( 115.3118051710478937, 82.87638965790608836, 147.0000028338058087 ) ) ;
#4858 = DIRECTION ( 'NONE',  ( 1.000000000000000000, 0.000000000000000000, -0.000000000000000000 ) ) ;
#4859 = EDGE_CURVE ( 'NONE', #4017, #341, #612, .T. ) ;
#4860 = DIRECTION ( 'NONE',  ( -2.295390878742131754E-32, 1.239088197126290570E-16, -1.000000000000000000 ) ) ;
#4861 = DIRECTION ( 'NONE',  ( -1.000000000000000000, 1.224646799147352468E-16, 0.000000000000000000 ) ) ;
#4862 = ORIENTED_EDGE ( 'NONE', *, *, #3017, .F. ) ;
#4863 =( LENGTH_UNIT ( ) NAMED_UNIT ( * ) SI_UNIT ( .MILLI., .METRE. ) );
#4864 = CIRCLE ( 'NONE', #350, 90.00000000000319744 ) ;
#4865 = FACE_OUTER_BOUND ( 'NONE', #4651, .T. ) ;
#4866 = ADVANCED_FACE ( 'NONE', ( #4364, #1402 ), #3363, .T. ) ;
#4867 = CARTESIAN_POINT ( 'NONE',  ( 73.99999999999987210, 76.99999716619419132, 5.000000000000000000 ) ) ;
#4868 = DIRECTION ( 'NONE',  ( 1.000000000000000000, 0.000000000000000000, -0.000000000000000000 ) ) ;
#4869 = ORIENTED_EDGE ( 'NONE', *, *, #1789, .T. ) ;
#4870 = LINE ( 'NONE', #2360, #1101 ) ;
#4871 = EDGE_CURVE ( 'NONE', #5642, #6227, #1440, .T. ) ;
#4872 = VERTEX_POINT ( 'NONE', #2912 ) ;
#4873 = CARTESIAN_POINT ( 'NONE',  ( -2.450350183182338881, 22.87332759541404670, 38.87800362567253387 ) ) ;
#4874 = EDGE_CURVE ( 'NONE', #1470, #554, #4885, .T. ) ;
#4875 = DIRECTION ( 'NONE',  ( -1.000000000000000000, -1.852483853906148286E-16, 0.000000000000000000 ) ) ;
#4876 = CARTESIAN_POINT ( 'NONE',  ( -0.2052511266214760433, -21.25619793154163517, -110.0000000000000000 ) ) ;
#4877 = LINE ( 'NONE', #5336, #2761 ) ;
#4878 = VERTEX_POINT ( 'NONE', #6213 ) ;
#4879 = EDGE_CURVE ( 'NONE', #4602, #4530, #1305, .T. ) ;
#4880 = ORIENTED_EDGE ( 'NONE', *, *, #521, .F. ) ;
#4881 = VERTEX_POINT ( 'NONE', #836 ) ;
#4882 = EDGE_LOOP ( 'NONE', ( #5215, #74, #5745, #186 ) ) ;
#4883 = EDGE_CURVE ( 'NONE', #5038, #861, #4416, .T. ) ;
#4884 = CARTESIAN_POINT ( 'NONE',  ( -22.00000000000000000, 0.000000000000000000, 47.00000000000000711 ) ) ;
#4885 = LINE ( 'NONE', #478, #5452 ) ;
#4886 = EDGE_CURVE ( 'NONE', #990, #1906, #516, .T. ) ;
#4887 = CARTESIAN_POINT ( 'NONE',  ( -10.97130857767021439, -22.47473234318869473, 6.237739505811241258 ) ) ;
#4888 = EDGE_LOOP ( 'NONE', ( #5403, #3384 ) ) ;
#4889 = DIRECTION ( 'NONE',  ( -1.000000000000000000, 0.000000000000000000, 0.000000000000000000 ) ) ;
#4890 = CARTESIAN_POINT ( 'NONE',  ( -3.065100562737908430, -22.79875969907089228, 24.91526600425119042 ) ) ;
#4891 = CARTESIAN_POINT ( 'NONE',  ( 6.500000000000001776, 120.0000000000000000, 12.00000000000000000 ) ) ;
#4892 = AXIS2_PLACEMENT_3D ( 'NONE', #5574, #98, #65 ) ;
#4893 = APPLICATION_CONTEXT ( 'automotive_design' ) ;
#4894 = DIRECTION ( 'NONE',  ( 1.224646799147353207E-16, 1.000000000000000000, -0.000000000000000000 ) ) ;
#4895 = ORIENTED_EDGE ( 'NONE', *, *, #5833, .T. ) ;
#4896 = AXIS2_PLACEMENT_3D ( 'NONE', #120, #2194, #5519 ) ;
#4897 = LINE ( 'NONE', #555, #2244 ) ;
#4898 = DIRECTION ( 'NONE',  ( -1.000000000000000000, 0.000000000000000000, 0.000000000000000000 ) ) ;
#4899 = DIRECTION ( 'NONE',  ( 0.000000000000000000, 0.000000000000000000, 1.000000000000000000 ) ) ;
#4900 = CARTESIAN_POINT ( 'NONE',  ( 0.000000000000000000, 0.000000000000000000, -49.99999999999999289 ) ) ;
#4901 =( GEOMETRIC_REPRESENTATION_CONTEXT ( 3 ) GLOBAL_UNCERTAINTY_ASSIGNED_CONTEXT ( ( #5668 ) ) GLOBAL_UNIT_ASSIGNED_CONTEXT ( ( #3147, #714, #3660 ) ) REPRESENTATION_CONTEXT ( 'NONE', 'WORKASPACE' ) );
#4902 = DIRECTION ( 'NONE',  ( 0.000000000000000000, 1.000000000000000000, 0.000000000000000000 ) ) ;
#4903 = ORIENTED_EDGE ( 'NONE', *, *, #2870, .F. ) ;
#4904 = CARTESIAN_POINT ( 'NONE',  ( 6.012884121744077603, 22.20400618356517697, 8.958536348443306707 ) ) ;
#4905 = CARTESIAN_POINT ( 'NONE',  ( 12.72356008887154211, 29.12127642700182051, 9.800582165931864154 ) ) ;
#4906 = DIRECTION ( 'NONE',  ( 1.000000000000000000, 0.000000000000000000, 0.000000000000000000 ) ) ;
#4907 = CARTESIAN_POINT ( 'NONE',  ( 0.000000000000000000, 0.000000000000000000, -273.0000000000000000 ) ) ;
#4908 = CIRCLE ( 'NONE', #4701, 90.00000000000319744 ) ;
#4909 = DIRECTION ( 'NONE',  ( 0.000000000000000000, 0.000000000000000000, 1.000000000000000000 ) ) ;
#4910 = DIRECTION ( 'NONE',  ( -0.000000000000000000, -0.000000000000000000, -1.000000000000000000 ) ) ;
#4911 = EDGE_LOOP ( 'NONE', ( #4296, #5209, #1271, #560 ) ) ;
#4912 = EDGE_LOOP ( 'NONE', ( #5132, #3200, #1925, #4595 ) ) ;
#4913 = VERTEX_POINT ( 'NONE', #5522 ) ;
#4914 = AXIS2_PLACEMENT_3D ( 'NONE', #615, #4525, #4014 ) ;
#4915 = ORIENTED_EDGE ( 'NONE', *, *, #473, .T. ) ;
#4916 = DIRECTION ( 'NONE',  ( -0.000000000000000000, -0.000000000000000000, -1.000000000000000000 ) ) ;
#4917 = DIRECTION ( 'NONE',  ( -0.000000000000000000, 0.000000000000000000, 1.000000000000000000 ) ) ;
#4918 = AXIS2_PLACEMENT_3D ( 'NONE', #1014, #2974, #5917 ) ;
#4919 = FACE_OUTER_BOUND ( 'NONE', #3093, .T. ) ;
#4920 = VERTEX_POINT ( 'NONE', #5439 ) ;
#4921 = CIRCLE ( 'NONE', #1940, 20.00000000000000000 ) ;
#4922 = DIRECTION ( 'NONE',  ( 0.000000000000000000, 0.000000000000000000, 1.000000000000000000 ) ) ;
#4923 = DIRECTION ( 'NONE',  ( -1.000000000000000000, -2.668808879446237100E-17, 0.000000000000000000 ) ) ;
#4924 = CARTESIAN_POINT ( 'NONE',  ( -0.4497881292104084494, -22.99670767401471849, 24.28508774596658526 ) ) ;
#4925 = CYLINDRICAL_SURFACE ( 'NONE', #2948, 22.67164836619068424 ) ;
#4926 = AXIS2_PLACEMENT_3D ( 'NONE', #1519, #4937, #2035 ) ;
#4927 = DIRECTION ( 'NONE',  ( -1.000000000000000000, 0.000000000000000000, 0.000000000000000000 ) ) ;
#4928 = ORIENTED_EDGE ( 'NONE', *, *, #3411, .T. ) ;
#4929 = CARTESIAN_POINT ( 'NONE',  ( 21.00000000000000355, 2.571758278209442056E-15, 12.00000000000000000 ) ) ;
#4930 = VERTEX_POINT ( 'NONE', #1988 ) ;
#4931 = DIRECTION ( 'NONE',  ( -0.000000000000000000, -0.000000000000000000, -1.000000000000000000 ) ) ;
#4932 = VECTOR ( 'NONE', #962, 1000.000000000000000 ) ;
#4933 = LINE ( 'NONE', #1941, #1721 ) ;
#4934 = AXIS2_PLACEMENT_3D ( 'NONE', #631, #5888, #1579 ) ;
#4935 = DIRECTION ( 'NONE',  ( 1.000000000000000000, 0.000000000000000000, 0.000000000000000000 ) ) ;
#4936 = VERTEX_POINT ( 'NONE', #5469 ) ;
#4937 = DIRECTION ( 'NONE',  ( -2.295390878742131754E-32, 1.239088197126290570E-16, -1.000000000000000000 ) ) ;
#4938 = VERTEX_POINT ( 'NONE', #5043 ) ;
#4939 = CARTESIAN_POINT ( 'NONE',  ( -2.012341796004660122, 22.91179784512888773, 39.00000000000001421 ) ) ;
#4940 = AXIS2_PLACEMENT_3D ( 'NONE', #6350, #105, #70 ) ;
#4941 = ADVANCED_BREP_SHAPE_REPRESENTATION ( '', ( #365, #6349 ), #4174 ) ;
#4942 = CARTESIAN_POINT ( 'NONE',  ( 16.23652742703164620, 37.28747423195200383, 15.00000000000000000 ) ) ;
#4943 = PLANE ( 'NONE',  #3981 ) ;
#4944 = CARTESIAN_POINT ( 'NONE',  ( 0.000000000000000000, 0.000000000000000000, 47.00000000000000711 ) ) ;
#4945 = ORIENTED_EDGE ( 'NONE', *, *, #2656, .F. ) ;
#4946 = CIRCLE ( 'NONE', #735, 89.87058297576894006 ) ;
#4947 = ORIENTED_EDGE ( 'NONE', *, *, #264, .T. ) ;
#4948 = ORIENTED_EDGE ( 'NONE', *, *, #860, .F. ) ;
#4949 = ORIENTED_EDGE ( 'NONE', *, *, #1937, .F. ) ;
#4950 = AXIS2_PLACEMENT_3D ( 'NONE', #4363, #6333, #3639 ) ;
#4951 = CARTESIAN_POINT ( 'NONE',  ( 0.000000000000000000, 0.000000000000000000, -45.00000000000000000 ) ) ;
#4952 = EDGE_CURVE ( 'NONE', #647, #3460, #4399, .T. ) ;
#4953 = CARTESIAN_POINT ( 'NONE',  ( -3.081487911019577365E-30, 5.660601460262082306E-46, 281.0000000000000000 ) ) ;
#4954 = CARTESIAN_POINT ( 'NONE',  ( -6.685354258535096683, -24.10283321907681753, 8.717551967824457293 ) ) ;
#4955 = EDGE_CURVE ( 'NONE', #1278, #5526, #925, .T. ) ;
#4956 = VERTEX_POINT ( 'NONE', #3466 ) ;
#4957 = B_SPLINE_CURVE_WITH_KNOTS ( 'NONE', 3,
 ( #3941, #3005, #1520, #4970, #4905, #501, #536, #5946, #2420, #1553, #4423, #4384, #5914, #4994, #1491, #3487, #1010, #5458 ),
 .UNSPECIFIED., .F., .F.,
 ( 4, 2, 2, 2, 2, 2, 2, 2, 4 ),
 ( 0.000000000000000000, 0.0007936035350328099784, 0.001587207070065619957, 0.002380810605098429827, 0.003174414140131239914, 0.003968017675164050434, 0.004761621210196859653, 0.005555224745229667138, 0.006348828280262475490 ),
 .UNSPECIFIED. ) ;
#4958 = AXIS2_PLACEMENT_3D ( 'NONE', #3296, #857, #3321 ) ;
#4959 = CARTESIAN_POINT ( 'NONE',  ( -15.99408614349810698, 16.52843635781563592, 0.000000000000000000 ) ) ;
#4960 = CARTESIAN_POINT ( 'NONE',  ( 0.000000000000000000, 25.00000000000000000, 31.77501000028010125 ) ) ;
#4961 = VERTEX_POINT ( 'NONE', #3434 ) ;
#4962 = DIRECTION ( 'NONE',  ( 1.000000000000000000, 0.000000000000000000, 0.000000000000000000 ) ) ;
#4963 = DIRECTION ( 'NONE',  ( 1.000000000000000000, 0.000000000000000000, 0.000000000000000000 ) ) ;
#4964 = CARTESIAN_POINT ( 'NONE',  ( 6.507303803555983812, 24.13991014445887373, 28.01358234833885774 ) ) ;
#4965 = ADVANCED_FACE ( 'NONE', ( #25 ), #3014, .F. ) ;
#4966 = CARTESIAN_POINT ( 'NONE',  ( -12.72367524380681303, 29.12081030169100870, 2.199628915743095270 ) ) ;
#4967 = DIRECTION ( 'NONE',  ( 0.000000000000000000, -1.000000000000000000, -1.239088197126290570E-16 ) ) ;
#4968 = ORIENTED_EDGE ( 'NONE', *, *, #4353, .F. ) ;
#4969 = CARTESIAN_POINT ( 'NONE',  ( 11.95959904370095650, 19.64922365089178768, 5.386438528827848238 ) ) ;
#4970 = CARTESIAN_POINT ( 'NONE',  ( 12.66240722304475064, 29.37208741619408059, 9.875474163642433467 ) ) ;
#4971 = CARTESIAN_POINT ( 'NONE',  ( 25.00000000000000000, 3.061616997868383043E-15, 47.00000000000000711 ) ) ;
#4972 = FACE_OUTER_BOUND ( 'NONE', #95, .T. ) ;
#4973 = AXIS2_PLACEMENT_3D ( 'NONE', #1843, #5166, #5783 ) ;
#4974 = DIRECTION ( 'NONE',  ( -0.000000000000000000, 0.000000000000000000, -1.000000000000000000 ) ) ;
#4975 = DIRECTION ( 'NONE',  ( -0.000000000000000000, 0.000000000000000000, -1.000000000000000000 ) ) ;
#4976 = VERTEX_POINT ( 'NONE', #4980 ) ;
#4977 = ORIENTED_EDGE ( 'NONE', *, *, #125, .F. ) ;
#4978 = ORIENTED_EDGE ( 'NONE', *, *, #1600, .F. ) ;
#4979 = DIRECTION ( 'NONE',  ( 0.000000000000000000, 1.000000000000000000, -0.000000000000000000 ) ) ;
#4980 = CARTESIAN_POINT ( 'NONE',  ( 22.00000000000000000, 2.694222958124176809E-15, 47.00000000000000711 ) ) ;
#4981 = CARTESIAN_POINT ( 'NONE',  ( -15.22537606545851396, -19.83673216789829397, 1.447296480073240410 ) ) ;
#4982 = ORIENTED_EDGE ( 'NONE', *, *, #1486, .T. ) ;
#4983 = DIRECTION ( 'NONE',  ( 4.776461258714217944E-16, 0.000000000000000000, 1.000000000000000222 ) ) ;
#4984 = CARTESIAN_POINT ( 'NONE',  ( -7.182657412981705209E-17, 20.00000000000000711, 39.27501000028011902 ) ) ;
#4985 = CYLINDRICAL_SURFACE ( 'NONE', #3598, 22.67164836619070911 ) ;
#4986 = ORIENTED_EDGE ( 'NONE', *, *, #3806, .F. ) ;
#4987 = CARTESIAN_POINT ( 'NONE',  ( -0.2052511266214760433, -21.25619793154163517, -175.0000000000000284 ) ) ;
#4988 = LINE ( 'NONE', #3511, #3652 ) ;
#4989 = DIRECTION ( 'NONE',  ( 1.000000000000000000, 0.000000000000000000, 0.000000000000000000 ) ) ;
#4990 = VECTOR ( 'NONE', #3019, 1000.000000000000000 ) ;
#4991 = CARTESIAN_POINT ( 'NONE',  ( 0.000000000000000000, 25.00000000000000000, 0.000000000000000000 ) ) ;
#4992 = ORIENTED_EDGE ( 'NONE', *, *, #100, .T. ) ;
#4993 = CARTESIAN_POINT ( 'NONE',  ( 13.14183123006966980, -39.58265509608656174, -130.0000000000000000 ) ) ;
#4994 = CARTESIAN_POINT ( 'NONE',  ( 13.35972283035915531, 26.60564881331300668, 7.306817940158689240 ) ) ;
#4995 = AXIS2_PLACEMENT_3D ( 'NONE', #4565, #4501, #3599 ) ;
#4996 = CARTESIAN_POINT ( 'NONE',  ( -7.199721615955812837, 21.84420850452976026, 33.88807004839755166 ) ) ;
#4997 = DIRECTION ( 'NONE',  ( -3.903561672282191229E-16, 1.000000000000000000, 0.000000000000000000 ) ) ;
#4998 = DIRECTION ( 'NONE',  ( 0.000000000000000000, 1.000000000000000000, 1.247733429937938623E-16 ) ) ;
#4999 = VERTEX_POINT ( 'NONE', #5988 ) ;
#5000 = ORIENTED_EDGE ( 'NONE', *, *, #5504, .F. ) ;
#5001 = AXIS2_PLACEMENT_3D ( 'NONE', #5276, #4748, #4780 ) ;
#5002 = VECTOR ( 'NONE', #4231, 1000.000000000000000 ) ;
#5003 = VERTEX_POINT ( 'NONE', #1474 ) ;
#5004 = CARTESIAN_POINT ( 'NONE',  ( -8.000000000000000000, 110.3953136438507130, 12.00000000000000000 ) ) ;
#5005 = CARTESIAN_POINT ( 'NONE',  ( 13.15471301119415770, 27.39842886758933105, 3.337628543836456796 ) ) ;
#5006 = LINE ( 'NONE', #5494, #6066 ) ;
#5007 = CIRCLE ( 'NONE', #3358, 21.00000000000000355 ) ;
#5008 = CARTESIAN_POINT ( 'NONE',  ( 8.000000000000007105, 72.93807001241029297, 12.00000000000000000 ) ) ;
#5009 = ORIENTED_EDGE ( 'NONE', *, *, #3933, .F. ) ;
#5010 = PRODUCT_DEFINITION_CONTEXT ( 'detailed design', #167, 'design' ) ;
#5011 =( REPRESENTATION_RELATIONSHIP ('NONE','NONE', #632, #5199 ) REPRESENTATION_RELATIONSHIP_WITH_TRANSFORMATION ( #5692 )SHAPE_REPRESENTATION_RELATIONSHIP( ) );
#5012 = VECTOR ( 'NONE', #3909, 1000.000000000000000 ) ;
#5013 = CARTESIAN_POINT ( 'NONE',  ( 72.31180517104782268, 82.87638965790611678, 249.4579780890716165 ) ) ;
#5014 = CARTESIAN_POINT ( 'NONE',  ( 0.000000000000000000, 0.000000000000000000, 48.00000000000000000 ) ) ;
#5015 = EDGE_CURVE ( 'NONE', #3955, #2906, #2456, .T. ) ;
#5016 = DIRECTION ( 'NONE',  ( 1.000000000000000000, 0.000000000000000000, 0.000000000000000000 ) ) ;
#5017 = VERTEX_POINT ( 'NONE', #3920 ) ;
#5018 = ORIENTED_EDGE ( 'NONE', *, *, #6162, .T. ) ;
#5019 = VECTOR ( 'NONE', #5291, 1000.000000000000000 ) ;
#5020 = CARTESIAN_POINT ( 'NONE',  ( -3.061616997868383043E-15, -25.00000000000000000, -130.0000000000000000 ) ) ;
#5021 = AXIS2_PLACEMENT_3D ( 'NONE', #2442, #4444, #2511 ) ;
#5022 = ADVANCED_FACE ( 'NONE', ( #6014 ), #3529, .T. ) ;
#5023 = LINE ( 'NONE', #2091, #5338 ) ;
#5024 = EDGE_CURVE ( 'NONE', #3628, #4645, #4306, .T. ) ;
#5025 = CYLINDRICAL_SURFACE ( 'NONE', #6281, 166.8359700257217071 ) ;
#5026 = EDGE_LOOP ( 'NONE', ( #4498, #5762, #5779, #6082 ) ) ;
#5027 = CARTESIAN_POINT ( 'NONE',  ( 16.23652742703164975, 37.28747423195200383, -45.00000000000000000 ) ) ;
#5028 = EDGE_CURVE ( 'NONE', #1742, #5434, #205, .T. ) ;
#5029 = AXIS2_PLACEMENT_3D ( 'NONE', #274, #4619, #3681 ) ;
#5030 = CARTESIAN_POINT ( 'NONE',  ( 6.807437345657000094, 21.96969009462961253, 34.93075177053970748 ) ) ;
#5031 = ADVANCED_FACE ( 'NONE', ( #5955 ), #5894, .T. ) ;
#5032 = EDGE_CURVE ( 'NONE', #5651, #5613, #5654, .T. ) ;
#5033 = CIRCLE ( 'NONE', #2861, 20.00000000000000000 ) ;
#5034 = CARTESIAN_POINT ( 'NONE',  ( 8.206466222643914676, 23.61787042823059224, 7.999630148859496970 ) ) ;
#5035 = VECTOR ( 'NONE', #6204, 1000.000000000000000 ) ;
#5036 = DIRECTION ( 'NONE',  ( -0.000000000000000000, -0.000000000000000000, -1.000000000000000000 ) ) ;
#5037 = ORIENTED_EDGE ( 'NONE', *, *, #29, .F. ) ;
#5038 = VERTEX_POINT ( 'NONE', #2047 ) ;
#5039 = ORIENTED_EDGE ( 'NONE', *, *, #865, .F. ) ;
#5040 = AXIS2_PLACEMENT_3D ( 'NONE', #4540, #1951, #4027 ) ;
#5041 = CARTESIAN_POINT ( 'NONE',  ( -22.21770253897231839, -3.871672004621880436, -240.0000000000000000 ) ) ;
#5042 = CARTESIAN_POINT ( 'NONE',  ( 12.47907056128239667, 30.13454381782201352, 1.999999999999989120 ) ) ;
#5043 = CARTESIAN_POINT ( 'NONE',  ( -17.00000000000000000, 25.00000000000000000, -225.0000000000000000 ) ) ;
#5044 = EDGE_CURVE ( 'NONE', #4328, #157, #2524, .T. ) ;
#5045 = VECTOR ( 'NONE', #2566, 1000.000000000000000 ) ;
#5046 = CARTESIAN_POINT ( 'NONE',  ( -44.43364355155666345, 29.42304313293565343, -160.0000000000000284 ) ) ;
#5047 = CARTESIAN_POINT ( 'NONE',  ( 17.00000000000000000, 2.081899558550500280E-15, 48.00000000000000000 ) ) ;
#5048 = ORIENTED_EDGE ( 'NONE', *, *, #4751, .F. ) ;
#5049 = CIRCLE ( 'NONE', #2261, 72.49991987048069575 ) ;
#5050 = CONTEXT_DEPENDENT_SHAPE_REPRESENTATION ( #5472, #665 ) ;
#5051 = SHAPE_DEFINITION_REPRESENTATION ( #6058, #632 ) ;
#5052 = CARTESIAN_POINT ( 'NONE',  ( 0.000000000000000000, 0.000000000000000000, 1.000000000000000888 ) ) ;
#5053 = AXIS2_PLACEMENT_3D ( 'NONE', #4143, #206, #1609 ) ;
#5054 = AXIS2_PLACEMENT_3D ( 'NONE', #2616, #2104, #1533 ) ;
#5055 = ORIENTED_EDGE ( 'NONE', *, *, #4758, .T. ) ;
#5056 = CARTESIAN_POINT ( 'NONE',  ( 279.0000000000000000, 14.00000000000000000, 0.000000000000000000 ) ) ;
#5057 = VERTEX_POINT ( 'NONE', #85 ) ;
#5058 = DIRECTION ( 'NONE',  ( 0.000000000000000000, 0.000000000000000000, 1.000000000000000000 ) ) ;
#5059 = EDGE_CURVE ( 'NONE', #1760, #4920, #5006, .T. ) ;
#5060 = DIRECTION ( 'NONE',  ( 0.000000000000000000, -0.000000000000000000, 1.000000000000000000 ) ) ;
#5061 = DIRECTION ( 'NONE',  ( 1.000000000000000000, 0.000000000000000000, -0.000000000000000000 ) ) ;
#5062 = ORIENTED_EDGE ( 'NONE', *, *, #3533, .F. ) ;
#5063 = DIRECTION ( 'NONE',  ( -0.000000000000000000, -0.000000000000000000, -1.000000000000000000 ) ) ;
#5064 = EDGE_CURVE ( 'NONE', #371, #6227, #1025, .T. ) ;
#5065 = LINE ( 'NONE', #1576, #3714 ) ;
#5066 = CARTESIAN_POINT ( 'NONE',  ( 6.497654244294650105, 22.06338186837085402, 35.52745571863555085 ) ) ;
#5067 = CARTESIAN_POINT ( 'NONE',  ( 15.63352991451900920, 19.51442596162454990, 0.7402269581920428720 ) ) ;
#5068 = DIRECTION ( 'NONE',  ( 0.000000000000000000, 0.000000000000000000, -1.000000000000000000 ) ) ;
#5069 = EDGE_CURVE ( 'NONE', #5434, #760, #4033, .T. ) ;
#5070 = EDGE_LOOP ( 'NONE', ( #1110, #2114, #1825, #4294 ) ) ;
#5071 = ORIENTED_EDGE ( 'NONE', *, *, #4184, .T. ) ;
#5072 = EDGE_CURVE ( 'NONE', #1184, #341, #2947, .T. ) ;
#5073 = ORIENTED_EDGE ( 'NONE', *, *, #4679, .T. ) ;
#5074 = DIRECTION ( 'NONE',  ( 1.000000000000000000, 0.000000000000000000, 0.000000000000000000 ) ) ;
#5075 = AXIS2_PLACEMENT_3D ( 'NONE', #2149, #3479, #4963 ) ;
#5076 = CARTESIAN_POINT ( 'NONE',  ( 13.38023260448823848, 26.52727575619375244, 4.947004611186090806 ) ) ;
#5077 = DIRECTION ( 'NONE',  ( 0.000000000000000000, 0.000000000000000000, -1.000000000000000000 ) ) ;
#5078 = EDGE_CURVE ( 'NONE', #5103, #4515, #764, .T. ) ;
#5079 = CARTESIAN_POINT ( 'NONE',  ( 67.00000000000000000, 69.00000000000000000, 110.0000000000000000 ) ) ;
#5080 = CARTESIAN_POINT ( 'NONE',  ( 82.00000000000001421, 69.00000000000000000, 110.0000000000000000 ) ) ;
#5081 = EDGE_LOOP ( 'NONE', ( #5449, #4040, #4053, #317 ) ) ;
#5082 = PRODUCT_RELATED_PRODUCT_CATEGORY ( 'part', '', ( #3229 ) ) ;
#5083 = LINE ( 'NONE', #90, #5568 ) ;
#5084 = EDGE_CURVE ( 'NONE', #2034, #5651, #5968, .T. ) ;
#5085 = SHAPE_DEFINITION_REPRESENTATION ( #6113, #5199 ) ;
#5086 = CARTESIAN_POINT ( 'NONE',  ( -6.807437345657000094, -21.96969009462961253, 34.93075177053970748 ) ) ;
#5087 = ORIENTED_EDGE ( 'NONE', *, *, #1996, .T. ) ;
#5088 = PRODUCT_DEFINITION_SHAPE ( 'NONE', 'NONE',  #3336 ) ;
#5089 = DIRECTION ( 'NONE',  ( -1.000000000000000000, 0.000000000000000000, 0.000000000000000000 ) ) ;
#5090 = VERTEX_POINT ( 'NONE', #1198 ) ;
#5091 = VERTEX_POINT ( 'NONE', #2852 ) ;
#5092 = DIRECTION ( 'NONE',  ( 0.000000000000000000, 0.000000000000000000, -1.000000000000000000 ) ) ;
#5093 = CARTESIAN_POINT ( 'NONE',  ( 0.000000000000000000, 0.000000000000000000, 51.00000000000002842 ) ) ;
#5094 = DIRECTION ( 'NONE',  ( -1.000000000000000000, 0.000000000000000000, 0.000000000000000000 ) ) ;
#5095 = CARTESIAN_POINT ( 'NONE',  ( -20.00000000000000000, 0.000000000000000000, 39.00000000000001421 ) ) ;
#5096 = ORIENTED_EDGE ( 'NONE', *, *, #1436, .T. ) ;
#5097 = DIRECTION ( 'NONE',  ( -1.000000000000000000, 0.000000000000000000, 0.000000000000000000 ) ) ;
#5098 = DIRECTION ( 'NONE',  ( -0.000000000000000000, -0.000000000000000000, -1.000000000000000000 ) ) ;
#5099 = CARTESIAN_POINT ( 'NONE',  ( -6.801000575755121069, 21.97168837322005075, 28.60528907419297084 ) ) ;
#5100 = CARTESIAN_POINT ( 'NONE',  ( -3.487686359055458762, 24.77054744280749077, 9.676329747922174818 ) ) ;
#5101 = CARTESIAN_POINT ( 'NONE',  ( 5.576854706809766249, -22.31420130230918986, 36.79476692679597249 ) ) ;
#5102 = AXIS2_PLACEMENT_3D ( 'NONE', #1484, #6321, #4898 ) ;
#5103 = VERTEX_POINT ( 'NONE', #6078 ) ;
#5104 = EDGE_CURVE ( 'NONE', #5616, #2301, #3175, .T. ) ;
#5105 = VERTEX_POINT ( 'NONE', #1712 ) ;
#5106 = CARTESIAN_POINT ( 'NONE',  ( 0.000000000000000000, 25.00000000000000000, -30.00000000000000000 ) ) ;
#5107 = CARTESIAN_POINT ( 'NONE',  ( 44.64065620456912598, 28.99954194078667413, -160.0000000000000284 ) ) ;
#5108 = CARTESIAN_POINT ( 'NONE',  ( 18.00000000000001421, 26.39531364385072010, 5.999999999999990230 ) ) ;
#5109 = PLANE ( 'NONE',  #4095 ) ;
#5110 = VECTOR ( 'NONE', #6301, 1000.000000000000000 ) ;
#5111 = AXIS2_PLACEMENT_3D ( 'NONE', #3308, #966, #4792 ) ;
#5112 = CARTESIAN_POINT ( 'NONE',  ( 0.000000000000000000, 25.00000000000000000, 301.0000000000000568 ) ) ;
#5113 = ORIENTED_EDGE ( 'NONE', *, *, #3629, .F. ) ;
#5114 = CARTESIAN_POINT ( 'NONE',  ( 6.500000000000000000, 134.5953136438507158, 12.00000000000000000 ) ) ;
#5115 = VECTOR ( 'NONE', #1586, 1000.000000000000000 ) ;
#5116 = ORIENTED_EDGE ( 'NONE', *, *, #3127, .T. ) ;
#5117 = CARTESIAN_POINT ( 'NONE',  ( -12.50000000000001421, 120.0000000000000000, 16.00000000000000000 ) ) ;
#5118 = ORIENTED_EDGE ( 'NONE', *, *, #3925, .F. ) ;
#5119 = VECTOR ( 'NONE', #1748, 1000.000000000000000 ) ;
#5120 = DIRECTION ( 'NONE',  ( 1.000000000000000000, 0.000000000000000000, 0.000000000000000000 ) ) ;
#5121 = DIRECTION ( 'NONE',  ( 0.000000000000000000, 0.000000000000000000, 1.000000000000000000 ) ) ;
#5122 = CARTESIAN_POINT ( 'NONE',  ( -22.00000000000000000, 0.000000000000000000, 41.00000000000000000 ) ) ;
#5123 = VECTOR ( 'NONE', #2062, 1000.000000000000000 ) ;
#5124 = CARTESIAN_POINT ( 'NONE',  ( 6.500000000000000000, 134.5953136438507158, 12.00000000000000000 ) ) ;
#5125 = ORIENTED_EDGE ( 'NONE', *, *, #6249, .F. ) ;
#5126 = CARTESIAN_POINT ( 'NONE',  ( -6.736606839469455821, 22.00628563274161920, 8.696944893850881542 ) ) ;
#5127 = DIRECTION ( 'NONE',  ( -1.000000000000000000, 0.000000000000000000, 0.000000000000000000 ) ) ;
#5128 = CARTESIAN_POINT ( 'NONE',  ( 2.380270672502711906E-15, -5.204170427930421283E-15, -30.00000000000000000 ) ) ;
#5129 = AXIS2_PLACEMENT_3D ( 'NONE', #5367, #5813, #4843 ) ;
#5130 = CARTESIAN_POINT ( 'NONE',  ( 13.84152781008414301, 20.82799749684992108, 3.414623522204560668 ) ) ;
#5131 = DIRECTION ( 'NONE',  ( -0.000000000000000000, -0.000000000000000000, -1.000000000000000000 ) ) ;
#5132 = ORIENTED_EDGE ( 'NONE', *, *, #32, .T. ) ;
#5133 =( GEOMETRIC_REPRESENTATION_CONTEXT ( 3 ) GLOBAL_UNCERTAINTY_ASSIGNED_CONTEXT ( ( #6117 ) ) GLOBAL_UNIT_ASSIGNED_CONTEXT ( ( #4863, #335, #4737 ) ) REPRESENTATION_CONTEXT ( 'NONE', 'WORKASPACE' ) );
#5134 = ORIENTED_EDGE ( 'NONE', *, *, #47, .T. ) ;
#5135 = LINE ( 'NONE', #1196, #479 ) ;
#5136 = VECTOR ( 'NONE', #5248, 1000.000000000000000 ) ;
#5137 = PRODUCT_DEFINITION_SHAPE ( 'NONE', 'NONE',  #6373 ) ;
#5138 = DIRECTION ( 'NONE',  ( 1.000000000000000000, 0.000000000000000000, 0.000000000000000000 ) ) ;
#5139 = VECTOR ( 'NONE', #5594, 1000.000000000000000 ) ;
#5140 = CARTESIAN_POINT ( 'NONE',  ( -43.99999999999990052, 13.41640786499905147, -65.00000000000000000 ) ) ;
#5141 =( REPRESENTATION_RELATIONSHIP ('NONE','NONE', #632, #1490 ) REPRESENTATION_RELATIONSHIP_WITH_TRANSFORMATION ( #3919 )SHAPE_REPRESENTATION_RELATIONSHIP( ) );
#5142 = LINE ( 'NONE', #4094, #619 ) ;
#5143 = VECTOR ( 'NONE', #3159, 1000.000000000000000 ) ;
#5144 = LINE ( 'NONE', #6296, #1528 ) ;
#5145 = ORIENTED_EDGE ( 'NONE', *, *, #4064, .T. ) ;
#5146 = EDGE_CURVE ( 'NONE', #2807, #4, #3722, .T. ) ;
#5147 = EDGE_CURVE ( 'NONE', #981, #3367, #569, .T. ) ;
#5148 = CARTESIAN_POINT ( 'NONE',  ( -3.061616997868383043E-15, -25.00000000000000000, -160.0000000000000000 ) ) ;
#5149 = VECTOR ( 'NONE', #6215, 1000.000000000000000 ) ;
#5150 = PRODUCT_CONTEXT ( 'NONE', #3699, 'mechanical' ) ;
#5151 = CARTESIAN_POINT ( 'NONE',  ( -9.051043717164153790, -21.15747665746626183, 7.546935333285830438 ) ) ;
#5152 = ORIENTED_EDGE ( 'NONE', *, *, #2011, .F. ) ;
#5153 = DIRECTION ( 'NONE',  ( -1.000000000000000000, 0.000000000000000000, 0.000000000000000000 ) ) ;
#5154 = CIRCLE ( 'NONE', #2471, 25.00000000000000000 ) ;
#5155 = EDGE_CURVE ( 'NONE', #4162, #5856, #5685, .T. ) ;
#5156 = VECTOR ( 'NONE', #5546, 1000.000000000000000 ) ;
#5157 = CIRCLE ( 'NONE', #5371, 90.00000000000000000 ) ;
#5158 = UNCERTAINTY_MEASURE_WITH_UNIT (LENGTH_MEASURE( 1.000000000000000082E-05 ), #5187, 'distance_accuracy_value', 'NONE');
#5159 = CARTESIAN_POINT ( 'NONE',  ( 7.947562104483774093, 68.75545066608756883, 1.999999999999994893 ) ) ;
#5160 = CARTESIAN_POINT ( 'NONE',  ( 0.000000000000000000, 25.00000000000000000, -195.0000000000000000 ) ) ;
#5161 = EDGE_CURVE ( 'NONE', #306, #5596, #3385, .T. ) ;
#5162 = DIRECTION ( 'NONE',  ( -0.000000000000000000, -0.000000000000000000, -1.000000000000000000 ) ) ;
#5163 = ORIENTED_EDGE ( 'NONE', *, *, #1261, .F. ) ;
#5164 = DIRECTION ( 'NONE',  ( -0.000000000000000000, 0.000000000000000000, 1.000000000000000000 ) ) ;
#5165 = DIRECTION ( 'NONE',  ( 0.000000000000000000, 1.000000000000000000, 0.000000000000000000 ) ) ;
#5166 = DIRECTION ( 'NONE',  ( -0.000000000000000000, -0.000000000000000000, -1.000000000000000000 ) ) ;
#5167 = EDGE_CURVE ( 'NONE', #6000, #775, #1431, .T. ) ;
#5168 = CIRCLE ( 'NONE', #3612, 19.00000000000000000 ) ;
#5169 = EDGE_CURVE ( 'NONE', #5213, #214, #2198, .T. ) ;
#5170 = CARTESIAN_POINT ( 'NONE',  ( -22.00000000000000000, 0.000000000000000000, 50.00000000000000711 ) ) ;
#5171 = CARTESIAN_POINT ( 'NONE',  ( 7.260561981364187290, -21.82400181508864634, 33.66843689838669462 ) ) ;
#5172 = ORIENTED_EDGE ( 'NONE', *, *, #196, .T. ) ;
#5173 = ORIENTED_EDGE ( 'NONE', *, *, #5288, .T. ) ;
#5174 = CARTESIAN_POINT ( 'NONE',  ( -7.451526880251365448, 23.86388513668106981, 30.79056676978084184 ) ) ;
#5175 = CARTESIAN_POINT ( 'NONE',  ( 67.00000000000000000, 69.00000000000000000, 0.000000000000000000 ) ) ;
#5176 = DIRECTION ( 'NONE',  ( 1.000000000000000000, 0.000000000000000000, 0.000000000000000000 ) ) ;
#5177 = DIRECTION ( 'NONE',  ( 0.000000000000000000, 0.000000000000000000, -1.000000000000000000 ) ) ;
#5178 = ORIENTED_EDGE ( 'NONE', *, *, #3013, .F. ) ;
#5179 = LINE ( 'NONE', #6175, #2346 ) ;
#5180 = ORIENTED_EDGE ( 'NONE', *, *, #1922, .F. ) ;
#5181 = AXIS2_PLACEMENT_3D ( 'NONE', #46, #4322, #2453 ) ;
#5182 = CARTESIAN_POINT ( 'NONE',  ( 7.500000000000000000, 9.184850993605147944E-16, 1.000000000000000888 ) ) ;
#5183 = CARTESIAN_POINT ( 'NONE',  ( -1.798140372219934502, -22.93384243835984648, 9.914400014297026331 ) ) ;
#5184 = VERTEX_POINT ( 'NONE', #1756 ) ;
#5185 = DIRECTION ( 'NONE',  ( 1.000000000000000000, 0.000000000000000000, -0.000000000000000000 ) ) ;
#5186 = ORIENTED_EDGE ( 'NONE', *, *, #118, .F. ) ;
#5187 =( LENGTH_UNIT ( ) NAMED_UNIT ( * ) SI_UNIT ( .MILLI., .METRE. ) );
#5188 = DIRECTION ( 'NONE',  ( -0.000000000000000000, 0.000000000000000000, -1.000000000000000000 ) ) ;
#5189 = DIRECTION ( 'NONE',  ( -0.000000000000000000, -0.000000000000000000, -1.000000000000000000 ) ) ;
#5190 = CARTESIAN_POINT ( 'NONE',  ( 0.000000000000000000, 25.00000000000000000, -30.00000000000000000 ) ) ;
#5191 = ORIENTED_EDGE ( 'NONE', *, *, #3748, .F. ) ;
#5192 = CARTESIAN_POINT ( 'NONE',  ( -13.86188709689055543, 18.36473791091104246, 3.388952392393740354 ) ) ;
#5193 = VERTEX_POINT ( 'NONE', #4059 ) ;
#5194 = CARTESIAN_POINT ( 'NONE',  ( 7.451677332883843263, 23.86383568307783065, 30.79254100948601547 ) ) ;
#5195 = CARTESIAN_POINT ( 'NONE',  ( 3.680439676527237136, 22.70725644061459647, 38.32515107347151684 ) ) ;
#5196 = DIRECTION ( 'NONE',  ( 1.000000000000000000, 0.000000000000000000, -0.000000000000000000 ) ) ;
#5197 = FACE_OUTER_BOUND ( 'NONE', #5787, .T. ) ;
#5198 = VERTEX_POINT ( 'NONE', #2617 ) ;
#5199 = SHAPE_REPRESENTATION ( 'Part 32,3_Varsay\X2\0131\X0\lan', ( #6349 ), #5524 ) ;
#5200 = ORIENTED_EDGE ( 'NONE', *, *, #4483, .F. ) ;
#5201 = CARTESIAN_POINT ( 'NONE',  ( -2.421623179306581441, 24.88356973210973777, 24.67241923065277831 ) ) ;
#5202 = SPHERICAL_SURFACE ( 'NONE', #797, 40.00000002749906258 ) ;
#5203 = DIRECTION ( 'NONE',  ( -0.000000000000000000, 0.000000000000000000, -1.000000000000000000 ) ) ;
#5204 = CIRCLE ( 'NONE', #476, 17.00000000000000000 ) ;
#5205 = FACE_OUTER_BOUND ( 'NONE', #1686, .T. ) ;
#5206 = CIRCLE ( 'NONE', #4896, 90.00000000000000000 ) ;
#5207 = ORIENTED_EDGE ( 'NONE', *, *, #23, .T. ) ;
#5208 = DIRECTION ( 'NONE',  ( -0.000000000000000000, -0.000000000000000000, -1.000000000000000000 ) ) ;
#5209 = ORIENTED_EDGE ( 'NONE', *, *, #5748, .T. ) ;
#5210 = CYLINDRICAL_SURFACE ( 'NONE', #1038, 17.00000000000000000 ) ;
#5211 = CARTESIAN_POINT ( 'NONE',  ( -11.04889961723839775, -20.18459349909284839, 6.176241220338072324 ) ) ;
#5212 = CIRCLE ( 'NONE', #485, 17.00000000000000000 ) ;
#5213 = VERTEX_POINT ( 'NONE', #5140 ) ;
#5214 = CARTESIAN_POINT ( 'NONE',  ( 64.99991398172927859, 0.000000000000000000, 281.0000000000000000 ) ) ;
#5215 = ORIENTED_EDGE ( 'NONE', *, *, #4286, .F. ) ;
#5216 = DIRECTION ( 'NONE',  ( -1.000000000000000000, 0.000000000000000000, 0.000000000000000000 ) ) ;
#5217 = AXIS2_PLACEMENT_3D ( 'NONE', #3180, #5601, #6146 ) ;
#5218 = CARTESIAN_POINT ( 'NONE',  ( 44.43364355155687662, -29.42304313293534790, -45.00000000000000000 ) ) ;
#5219 = DIRECTION ( 'NONE',  ( 0.000000000000000000, 0.000000000000000000, -1.000000000000000000 ) ) ;
#5220 = CARTESIAN_POINT ( 'NONE',  ( -0.9889208576060591893, -24.98510605705583387, 24.32423630022273286 ) ) ;
#5221 = ORIENTED_EDGE ( 'NONE', *, *, #3024, .T. ) ;
#5222 = AXIS2_PLACEMENT_3D ( 'NONE', #3956, #674, #4558 ) ;
#5223 = ORIENTED_EDGE ( 'NONE', *, *, #3619, .T. ) ;
#5224 = CARTESIAN_POINT ( 'NONE',  ( 7.114947004179564161, 23.96699118800356487, 34.19833922271499915 ) ) ;
#5225 = CARTESIAN_POINT ( 'NONE',  ( 42.00000000000000000, 69.00000000000000000, 110.0000000000000000 ) ) ;
#5226 = APPLICATION_CONTEXT ( 'automotive_design' ) ;
#5227 = EDGE_CURVE ( 'NONE', #3307, #1044, #3075, .T. ) ;
#5228 = VECTOR ( 'NONE', #1555, 1000.000000000000000 ) ;
#5229 = ADVANCED_FACE ( 'NONE', ( #2105 ), #1269, .T. ) ;
#5230 = DIRECTION ( 'NONE',  ( 0.000000000000000000, 0.000000000000000000, 1.000000000000000000 ) ) ;
#5232 = EDGE_CURVE ( 'NONE', #2249, #6115, #1950, .T. ) ;
#5231 = CARTESIAN_POINT ( 'NONE',  ( 0.4497709217647500868, -23.00000000000000355, 24.27501000028010836 ) ) ;
#5233 = ORIENTED_EDGE ( 'NONE', *, *, #5982, .F. ) ;
#5234 = ORIENTED_EDGE ( 'NONE', *, *, #5989, .T. ) ;
#5235 = CARTESIAN_POINT ( 'NONE',  ( -4.953009495843456733, 24.50520187577543396, 26.13782778128490136 ) ) ;
#5236 = EDGE_CURVE ( 'NONE', #4541, #738, #5551, .T. ) ;
#5237 = EDGE_CURVE ( 'NONE', #1266, #3016, #1621, .T. ) ;
#5238 = DIRECTION ( 'NONE',  ( -0.000000000000000000, -0.000000000000000000, -1.000000000000000000 ) ) ;
#5239 = CARTESIAN_POINT ( 'NONE',  ( 17.05141243254545458, -2.957948544529944430E-14, 12.00000000000000000 ) ) ;
#5240 =( GEOMETRIC_REPRESENTATION_CONTEXT ( 3 ) GLOBAL_UNCERTAINTY_ASSIGNED_CONTEXT ( ( #1733 ) ) GLOBAL_UNIT_ASSIGNED_CONTEXT ( ( #3154, #3313, #2893 ) ) REPRESENTATION_CONTEXT ( 'NONE', 'WORKASPACE' ) );
#5241 = DIRECTION ( 'NONE',  ( -0.000000000000000000, -0.000000000000000000, -1.000000000000000000 ) ) ;
#5242 = ORIENTED_EDGE ( 'NONE', *, *, #1148, .T. ) ;
#5243 = ORIENTED_EDGE ( 'NONE', *, *, #786, .F. ) ;
#5244 = AXIS2_PLACEMENT_3D ( 'NONE', #6334, #444, #2372 ) ;
#5245 = ADVANCED_FACE ( 'NONE', ( #1138 ), #2168, .F. ) ;
#5246 = CYLINDRICAL_SURFACE ( 'NONE', #329, 46.00000000000000000 ) ;
#5247 = CARTESIAN_POINT ( 'NONE',  ( 1.707452990153496275, -22.95315184250077323, 9.939577019203930774 ) ) ;
#5248 = DIRECTION ( 'NONE',  ( -0.000000000000000000, -0.000000000000000000, -1.000000000000000000 ) ) ;
#5249 = VECTOR ( 'NONE', #1857, 1000.000000000000000 ) ;
#5250 = EDGE_LOOP ( 'NONE', ( #2341, #1096, #3071, #6039 ) ) ;
#5251 = DIRECTION ( 'NONE',  ( -0.000000000000000000, -0.000000000000000000, 1.000000000000000000 ) ) ;
#5252 = ORIENTED_EDGE ( 'NONE', *, *, #1395, .F. ) ;
#5253 = VECTOR ( 'NONE', #2128, 1000.000000000000000 ) ;
#5254 = DIRECTION ( 'NONE',  ( -0.000000000000000000, -0.000000000000000000, 1.000000000000000000 ) ) ;
#5255 =( LENGTH_UNIT ( ) NAMED_UNIT ( * ) SI_UNIT ( .MILLI., .METRE. ) );
#5256 = CARTESIAN_POINT ( 'NONE',  ( 0.000000000000000000, 0.000000000000000000, -65.00000000000000000 ) ) ;
#5257 = DIRECTION ( 'NONE',  ( -1.000000000000000000, 0.000000000000000000, 0.000000000000000000 ) ) ;
#5258 = CIRCLE ( 'NONE', #2367, 46.00000000000000000 ) ;
#5259 = CARTESIAN_POINT ( 'NONE',  ( -5.958576596270774850, -24.28117850353844176, 27.19366677815228428 ) ) ;
#5260 = ORIENTED_EDGE ( 'NONE', *, *, #3629, .T. ) ;
#5261 = DIRECTION ( 'NONE',  ( -1.000000000000000000, -0.000000000000000000, -0.000000000000000000 ) ) ;
#5262 = ORIENTED_EDGE ( 'NONE', *, *, #4397, .T. ) ;
#5263 = EDGE_CURVE ( 'NONE', #3333, #5570, #4126, .T. ) ;
#5264 = CLOSED_SHELL ( 'NONE', ( #4192, #114, #3882, #3685, #2729, #1878, #2872, #1331, #1829, #3443, #506, #3330, #2943, #1357, #4104, #6064, #4009, #267, #1322, #2193, #3691, #5430, #76, #2585, #3742, #5700, #3255, #1127, #4779, #940, #1891, #1638, #4753, #6230, #3403 ) ) ;
#5265 = CARTESIAN_POINT ( 'NONE',  ( -15.82602517378898987, 37.28747423195201094, -240.0000000000000000 ) ) ;
#5266 = DIRECTION ( 'NONE',  ( 1.000000000000000000, 0.000000000000000000, 0.000000000000000000 ) ) ;
#5267 = CARTESIAN_POINT ( 'NONE',  ( -7.500000000000000000, 0.000000000000000000, 47.00000000000000000 ) ) ;
#5268 =( GEOMETRIC_REPRESENTATION_CONTEXT ( 3 ) GLOBAL_UNCERTAINTY_ASSIGNED_CONTEXT ( ( #1212 ) ) GLOBAL_UNIT_ASSIGNED_CONTEXT ( ( #3670, #173, #4081 ) ) REPRESENTATION_CONTEXT ( 'NONE', 'WORKASPACE' ) );
#5269 = CARTESIAN_POINT ( 'NONE',  ( 6.506525936991935488, -24.14011651440023698, 28.01231256153108973 ) ) ;
#5270 = EDGE_CURVE ( 'NONE', #3869, #4602, #3903, .T. ) ;
#5271 = VERTEX_POINT ( 'NONE', #2775 ) ;
#5272 = EDGE_CURVE ( 'NONE', #2635, #4666, #1822, .T. ) ;
#5273 = ORIENTED_EDGE ( 'NONE', *, *, #1834, .T. ) ;
#5274 = CARTESIAN_POINT ( 'NONE',  ( -7.101515257722369689, 23.97027555112600083, 29.35032263750040116 ) ) ;
#5275 = AXIS2_PLACEMENT_3D ( 'NONE', #4566, #5121, #2665 ) ;
#5276 = CARTESIAN_POINT ( 'NONE',  ( 0.000000000000000000, 0.000000000000000000, 12.00000000000000000 ) ) ;
#5277 = PLANE ( 'NONE',  #6256 ) ;
#5278 = EDGE_CURVE ( 'NONE', #5632, #414, #1856, .T. ) ;
#5279 = CYLINDRICAL_SURFACE ( 'NONE', #3693, 89.99999999999998579 ) ;
#5280 = ORIENTED_EDGE ( 'NONE', *, *, #2532, .T. ) ;
#5281 = EDGE_LOOP ( 'NONE', ( #742, #2745, #5125, #6207 ) ) ;
#5282 = ORIENTED_EDGE ( 'NONE', *, *, #5456, .F. ) ;
#5283 = CARTESIAN_POINT ( 'NONE',  ( 44.00000000000008527, 13.41640786499836224, -175.0000000000000284 ) ) ;
#5284 = DIRECTION ( 'NONE',  ( -1.000000000000000000, 0.000000000000000000, 0.000000000000000000 ) ) ;
#5285 = PLANE ( 'NONE',  #111 ) ;
#5286 = VERTEX_POINT ( 'NONE', #2365 ) ;
#5287 = CARTESIAN_POINT ( 'NONE',  ( 16.00000000000000000, 1.959434878635765131E-15, 12.00000000000000000 ) ) ;
#5288 = EDGE_CURVE ( 'NONE', #4913, #5734, #5870, .T. ) ;
#5289 = DIRECTION ( 'NONE',  ( 1.391202364994600813E-15, 0.9868877816584250562, -0.1614078883243098006 ) ) ;
#5290 = CARTESIAN_POINT ( 'NONE',  ( 44.64065620456912598, 28.99954194078667413, -49.99999999999999289 ) ) ;
#5291 = DIRECTION ( 'NONE',  ( -0.000000000000000000, -0.000000000000000000, -1.000000000000000000 ) ) ;
#5292 = CARTESIAN_POINT ( 'NONE',  ( -0.4985038669289053592, -25.00000000000000000, 24.27501000028010480 ) ) ;
#5293 = EDGE_LOOP ( 'NONE', ( #1363, #971, #4476, #978 ) ) ;
#5294 = DIRECTION ( 'NONE',  ( -1.852483853906148040E-16, 1.000000000000000000, 1.239088197126290570E-16 ) ) ;
#5295 = CARTESIAN_POINT ( 'NONE',  ( 0.000000000000000000, 0.000000000000000000, 50.00000000000000711 ) ) ;
#5296 = PLANE ( 'NONE',  #3570 ) ;
#5297 = CARTESIAN_POINT ( 'NONE',  ( 5.951225761847369178, -24.28185285436556740, 36.34586759703543635 ) ) ;
#5298 = ORIENTED_EDGE ( 'NONE', *, *, #3532, .T. ) ;
#5299 = VERTEX_POINT ( 'NONE', #410 ) ;
#5300 = CARTESIAN_POINT ( 'NONE',  ( -3.329879077396675324, 24.78142485916625049, 38.51307783140498486 ) ) ;
#5301 = CARTESIAN_POINT ( 'NONE',  ( 16.23652742703164620, 37.28747423195200383, -240.0000000000000000 ) ) ;
#5302 = CARTESIAN_POINT ( 'NONE',  ( 44.00000000000009948, 13.41640786499835514, -115.0000000000000000 ) ) ;
#5303 = ADVANCED_FACE ( 'NONE', ( #2811 ), #3785, .T. ) ;
#5304 = FACE_BOUND ( 'NONE', #3003, .T. ) ;
#5305 = EDGE_LOOP ( 'NONE', ( #4736, #4524, #696, #4023 ) ) ;
#5306 = ORIENTED_EDGE ( 'NONE', *, *, #2848, .T. ) ;
#5307 = ORIENTED_EDGE ( 'NONE', *, *, #6304, .F. ) ;
#5308 = DIRECTION ( 'NONE',  ( -0.000000000000000000, -0.000000000000000000, -1.000000000000000000 ) ) ;
#5309 = CARTESIAN_POINT ( 'NONE',  ( -13.35972283035916774, 26.60564881331300668, 7.306817940158690128 ) ) ;
#5310 = EDGE_CURVE ( 'NONE', #2368, #661, #3881, .T. ) ;
#5311 = LINE ( 'NONE', #325, #5149 ) ;
#5312 = ORIENTED_EDGE ( 'NONE', *, *, #2923, .F. ) ;
#5313 = CIRCLE ( 'NONE', #4995, 16.00000000000000355 ) ;
#5314 = CARTESIAN_POINT ( 'NONE',  ( 8.000000000000021316, 1.729804722550182166E-15, 9.999999999999987566 ) ) ;
#5315 = EDGE_CURVE ( 'NONE', #1044, #3307, #2032, .T. ) ;
#5316 = EDGE_CURVE ( 'NONE', #1997, #2301, #5818, .T. ) ;
#5317 = DIRECTION ( 'NONE',  ( 1.425674875965643413E-16, 0.9868877816584197271, -0.1614078883243422469 ) ) ;
#5318 = CARTESIAN_POINT ( 'NONE',  ( -3.474965785108256267, -22.73929270720903872, 25.11363447059788712 ) ) ;
#5319 = DIRECTION ( 'NONE',  ( 1.000000000000000000, 0.000000000000000000, 0.000000000000000000 ) ) ;
#5320 = DIRECTION ( 'NONE',  ( 1.000000000000000000, 0.000000000000000000, 0.000000000000000000 ) ) ;
#5321 = ORIENTED_EDGE ( 'NONE', *, *, #2934, .T. ) ;
#5322 = AXIS2_PLACEMENT_3D ( 'NONE', #2647, #3196, #1166 ) ;
#5323 = CIRCLE ( 'NONE', #6136, 24.99999999999999289 ) ;
#5324 = DIRECTION ( 'NONE',  ( 0.000000000000000000, -0.000000000000000000, -1.000000000000000000 ) ) ;
#5325 = CARTESIAN_POINT ( 'NONE',  ( 19.00000000000000000, 0.000000000000000000, -248.0000000000000000 ) ) ;
#5326 = PLANE ( 'NONE',  #1936 ) ;
#5327 = AXIS2_PLACEMENT_3D ( 'NONE', #715, #3148, #3213 ) ;
#5328 = CARTESIAN_POINT ( 'NONE',  ( 7.269041597172756219, -21.82161019007790514, 29.87399971471650062 ) ) ;
#5329 = ORIENTED_EDGE ( 'NONE', *, *, #5986, .T. ) ;
#5330 = CARTESIAN_POINT ( 'NONE',  ( -16.23652742703190199, -37.28747423195189015, -49.99999999999999289 ) ) ;
#5331 = ORIENTED_EDGE ( 'NONE', *, *, #4952, .T. ) ;
#5332 = CARTESIAN_POINT ( 'NONE',  ( 0.000000000000000000, 0.000000000000000000, -49.99999999999999289 ) ) ;
#5333 = CIRCLE ( 'NONE', #3471, 17.00000000000000000 ) ;
#5334 = CARTESIAN_POINT ( 'NONE',  ( 2.546401178541497462E-16, 25.00000000000000000, 24.27501000028010125 ) ) ;
#5335 = DIRECTION ( 'NONE',  ( -0.000000000000000000, -0.000000000000000000, -1.000000000000000000 ) ) ;
#5336 = CARTESIAN_POINT ( 'NONE',  ( -12.50000000000000355, 120.0000000000000000, 12.00000000000000000 ) ) ;
#5337 = CIRCLE ( 'NONE', #293, 17.00000000000000000 ) ;
#5338 = VECTOR ( 'NONE', #622, 1000.000000000000000 ) ;
#5339 = ORIENTED_EDGE ( 'NONE', *, *, #4554, .T. ) ;
#5340 = ORIENTED_EDGE ( 'NONE', *, *, #1122, .F. ) ;
#5341 = EDGE_CURVE ( 'NONE', #3812, #5742, #1887, .T. ) ;
#5342 = PRESENTATION_LAYER_ASSIGNMENT (  '', '', ( #1210 ) ) ;
#5343 = CARTESIAN_POINT ( 'NONE',  ( 0.000000000000000000, 0.000000000000000000, 301.0000000000000568 ) ) ;
#5344 = CARTESIAN_POINT ( 'NONE',  ( -12.72356008887154033, 29.12127642700181340, 9.800582165931858825 ) ) ;
#5345 = CARTESIAN_POINT ( 'NONE',  ( -1.698285149303729868, -24.95717370495094301, 9.939986931234113143 ) ) ;
#5346 = VERTEX_POINT ( 'NONE', #1298 ) ;
#5347 = EDGE_CURVE ( 'NONE', #4878, #53, #4749, .T. ) ;
#5348 = AXIS2_PLACEMENT_3D ( 'NONE', #4245, #847, #2800 ) ;
#5349 = ITEM_DEFINED_TRANSFORMATION ( 'NONE', 'NONE', #4914,  #6349 ) ;
#5350 = CARTESIAN_POINT ( 'NONE',  ( 107.0000000000000142, 69.00000000000000000, 0.000000000000000000 ) ) ;
#5351 = DIRECTION ( 'NONE',  ( 0.000000000000000000, 0.000000000000000000, 1.000000000000000000 ) ) ;
#5352 = CARTESIAN_POINT ( 'NONE',  ( 6.500000000000000000, 0.000000000000000000, 12.00000000000000000 ) ) ;
#5353 = AXIS2_PLACEMENT_3D ( 'NONE', #2558, #4520, #2079 ) ;
#5354 = CARTESIAN_POINT ( 'NONE',  ( 18.00000000000000355, 100.3953136438507272, 10.00000000000000000 ) ) ;
#5355 = EDGE_CURVE ( 'NONE', #4976, #414, #504, .T. ) ;
#5356 = FACE_OUTER_BOUND ( 'NONE', #2291, .T. ) ;
#5357 = VERTEX_POINT ( 'NONE', #794 ) ;
#5358 = ADVANCED_FACE ( 'NONE', ( #2331 ), #4291, .T. ) ;
#5359 = PLANE ( 'NONE',  #5760 ) ;
#5360 = AXIS2_PLACEMENT_3D ( 'NONE', #1676, #3098, #1160 ) ;
#5361 = CYLINDRICAL_SURFACE ( 'NONE', #1589, 17.00000000000000000 ) ;
#5362 = PLANE ( 'NONE',  #2781 ) ;
#5363 = EDGE_CURVE ( 'NONE', #6115, #157, #5636, .T. ) ;
#5364 = CARTESIAN_POINT ( 'NONE',  ( -13.35991119780008773, 26.60492657425308138, 4.695075907386110359 ) ) ;
#5365 = CARTESIAN_POINT ( 'NONE',  ( 7.245258220727284204, -23.92722011157075457, 29.82133114287520215 ) ) ;
#5366 = EDGE_LOOP ( 'NONE', ( #815, #1952, #213, #2258 ) ) ;
#5367 = CARTESIAN_POINT ( 'NONE',  ( 0.000000000000000000, 0.000000000000000000, 15.00000000000000000 ) ) ;
#5368 = ORIENTED_EDGE ( 'NONE', *, *, #5715, .F. ) ;
#5369 = DIRECTION ( 'NONE',  ( -0.000000000000000000, -0.000000000000000000, -1.000000000000000000 ) ) ;
#5370 = ADVANCED_FACE ( 'NONE', ( #2874 ), #5277, .T. ) ;
#5371 = AXIS2_PLACEMENT_3D ( 'NONE', #4200, #3729, #803 ) ;
#5372 = DIRECTION ( 'NONE',  ( -1.000000000000000000, 0.000000000000000000, 0.000000000000000000 ) ) ;
#5373 = FACE_BOUND ( 'NONE', #1750, .T. ) ;
#5374 = FACE_OUTER_BOUND ( 'NONE', #260, .T. ) ;
#5375 = ORIENTED_EDGE ( 'NONE', *, *, #4058, .F. ) ;
#5376 = ORIENTED_EDGE ( 'NONE', *, *, #2859, .T. ) ;
#5377 = VERTEX_POINT ( 'NONE', #3266 ) ;
#5378 = DIRECTION ( 'NONE',  ( -1.000000000000000000, 0.000000000000000000, 0.000000000000000000 ) ) ;
#5379 = CARTESIAN_POINT ( 'NONE',  ( -13.15428815592194134, 27.40009807703880185, 8.663997969339835237 ) ) ;
#5380 = AXIS2_PLACEMENT_3D ( 'NONE', #2210, #6147, #1734 ) ;
#5381 = CARTESIAN_POINT ( 'NONE',  ( 5.542644329336980036, -24.38138258431391847, 9.119897054702292394 ) ) ;
#5382 = ORIENTED_EDGE ( 'NONE', *, *, #1801, .F. ) ;
#5383 = DIRECTION ( 'NONE',  ( -0.000000000000000000, -0.000000000000000000, -1.000000000000000000 ) ) ;
#5384 = CARTESIAN_POINT ( 'NONE',  ( 87.31180517104787953, 82.87638965790608836, 147.0000028338058087 ) ) ;
#5385 = CARTESIAN_POINT ( 'NONE',  ( -7.412736743525290883, -21.77298136741688950, 33.00284858769864371 ) ) ;
#5386 = CARTESIAN_POINT ( 'NONE',  ( 0.000000000000000000, 76.99999716619419132, 276.0000000000000000 ) ) ;
#5387 = DIRECTION ( 'NONE',  ( 0.000000000000000000, 0.000000000000000000, -1.000000000000000000 ) ) ;
#5388 = ORIENTED_EDGE ( 'NONE', *, *, #3991, .F. ) ;
#5389 = DIRECTION ( 'NONE',  ( -0.000000000000000000, -0.000000000000000000, -1.000000000000000000 ) ) ;
#5390 = VECTOR ( 'NONE', #367, 1000.000000000000000 ) ;
#5391 = CARTESIAN_POINT ( 'NONE',  ( -2.012341796004660122, 22.91179784512888773, 39.00000000000001421 ) ) ;
#5392 = DIRECTION ( 'NONE',  ( 1.000000000000000000, 0.000000000000000000, 0.000000000000000000 ) ) ;
#5393 = CARTESIAN_POINT ( 'NONE',  ( -13.00793927997763610, 27.97619002235531838, 2.803925835876298400 ) ) ;
#5394 = DIRECTION ( 'NONE',  ( 2.295390878742131754E-32, -1.239088197126290570E-16, 1.000000000000000000 ) ) ;
#5395 = ORIENTED_EDGE ( 'NONE', *, *, #3024, .F. ) ;
#5396 = ORIENTED_EDGE ( 'NONE', *, *, #1486, .F. ) ;
#5397 = DIRECTION ( 'NONE',  ( -1.000000000000000000, 0.000000000000000000, 0.000000000000000000 ) ) ;
#5398 = CARTESIAN_POINT ( 'NONE',  ( 0.000000000000000000, 0.000000000000000000, -240.0000000000000000 ) ) ;
#5399 = LINE ( 'NONE', #2039, #288 ) ;
#5400 = LINE ( 'NONE', #1983, #1220 ) ;
#5401 = ORIENTED_EDGE ( 'NONE', *, *, #2582, .F. ) ;
#5402 = ORIENTED_EDGE ( 'NONE', *, *, #6019, .F. ) ;
#5403 = ORIENTED_EDGE ( 'NONE', *, *, #3338, .F. ) ;
#5404 = ORIENTED_EDGE ( 'NONE', *, *, #3415, .F. ) ;
#5405 = PLANE ( 'NONE',  #1865 ) ;
#5406 = DIRECTION ( 'NONE',  ( 1.000000000000000000, 0.000000000000000000, 0.000000000000000000 ) ) ;
#5407 = DIRECTION ( 'NONE',  ( -1.000000000000000000, 0.000000000000000000, 0.000000000000000000 ) ) ;
#5408 = ORIENTED_EDGE ( 'NONE', *, *, #1913, .F. ) ;
#5409 = CARTESIAN_POINT ( 'NONE',  ( -22.21770253897231839, -3.871672004621880436, 15.00000000000000000 ) ) ;
#5410 = DIRECTION ( 'NONE',  ( -0.000000000000000000, -0.000000000000000000, -1.000000000000000000 ) ) ;
#5411 = FACE_BOUND ( 'NONE', #498, .T. ) ;
#5412 = VECTOR ( 'NONE', #3315, 1000.000000000000000 ) ;
#5413 = DIRECTION ( 'NONE',  ( -0.000000000000000000, -0.000000000000000000, -1.000000000000000000 ) ) ;
#5414 = ORIENTED_EDGE ( 'NONE', *, *, #40, .T. ) ;
#5415 = AXIS2_PLACEMENT_3D ( 'NONE', #2024, #3049, #5475 ) ;
#5416 = DIRECTION ( 'NONE',  ( -1.000000000000000000, 0.000000000000000000, 0.000000000000000000 ) ) ;
#5417 = DIRECTION ( 'NONE',  ( 1.000000000000000000, 0.000000000000000000, 0.000000000000000000 ) ) ;
#5418 = AXIS2_PLACEMENT_3D ( 'NONE', #2500, #4460, #1099 ) ;
#5419 = CARTESIAN_POINT ( 'NONE',  ( -12.89959272829392667, 28.40844700521620680, 2.518705683379065974 ) ) ;
#5420 = CIRCLE ( 'NONE', #383, 17.00000000000000000 ) ;
#5421 = FACE_OUTER_BOUND ( 'NONE', #2283, .T. ) ;
#5422 = ORIENTED_EDGE ( 'NONE', *, *, #679, .F. ) ;
#5423 = DIRECTION ( 'NONE',  ( -1.000000000000000000, 0.000000000000000000, 0.000000000000000000 ) ) ;
#5424 = EDGE_LOOP ( 'NONE', ( #3136, #1408, #5408, #3687, #2441, #1239, #4420, #884, #3773 ) ) ;
#5425 = FACE_OUTER_BOUND ( 'NONE', #1308, .T. ) ;
#5426 = EDGE_CURVE ( 'NONE', #1338, #2268, #3672, .T. ) ;
#5427 = EDGE_CURVE ( 'NONE', #4122, #4938, #5333, .T. ) ;
#5428 = FACE_BOUND ( 'NONE', #178, .T. ) ;
#5429 = CIRCLE ( 'NONE', #2124, 22.00000000000000000 ) ;
#5430 = ADVANCED_FACE ( 'NONE', ( #3322 ), #5852, .T. ) ;
#5431 = DIRECTION ( 'NONE',  ( -0.000000000000000000, -0.000000000000000000, 1.000000000000000000 ) ) ;
#5432 = FACE_OUTER_BOUND ( 'NONE', #4381, .T. ) ;
#5433 = ORIENTED_EDGE ( 'NONE', *, *, #3936, .F. ) ;
#5434 = VERTEX_POINT ( 'NONE', #5302 ) ;
#5435 = ORIENTED_EDGE ( 'NONE', *, *, #5902, .T. ) ;
#5436 = ADVANCED_FACE ( 'NONE', ( #4812 ), #598, .F. ) ;
#5437 = EDGE_CURVE ( 'NONE', #768, #5105, #704, .T. ) ;
#5438 = CARTESIAN_POINT ( 'NONE',  ( 12.66355262481067889, 29.36736923042837333, 2.125736663006382088 ) ) ;
#5439 = CARTESIAN_POINT ( 'NONE',  ( 8.000000000000005329, 110.3953136438506988, 0.000000000000000000 ) ) ;
#5440 = CIRCLE ( 'NONE', #2645, 25.00000000000000000 ) ;
#5441 = CARTESIAN_POINT ( 'NONE',  ( 7.127827911436781072, -23.96564785266028963, 8.515057432034144114 ) ) ;
#5442 = ORIENTED_EDGE ( 'NONE', *, *, #2499, .T. ) ;
#5443 = ADVANCED_FACE ( 'NONE', ( #1068 ), #1495, .F. ) ;
#5444 = AXIS2_PLACEMENT_3D ( 'NONE', #220, #1587, #1563 ) ;
#5445 = PRODUCT_CONTEXT ( 'NONE', #5226, 'mechanical' ) ;
#5446 = PLANE ( 'NONE',  #4533 ) ;
#5447=STYLED_ITEM('',(#6419),#4609);
#5448 = FACE_BOUND ( 'NONE', #6241, .T. ) ;
#5449 = ORIENTED_EDGE ( 'NONE', *, *, #4682, .F. ) ;
#5450 = CARTESIAN_POINT ( 'NONE',  ( 0.000000000000000000, 0.000000000000000000, 23.00000000000000000 ) ) ;
#5451 = LINE ( 'NONE', #6024, #6025 ) ;
#5452 = VECTOR ( 'NONE', #2433, 1000.000000000000000 ) ;
#5453 = DIRECTION ( 'NONE',  ( -1.000000000000000000, -0.000000000000000000, -0.000000000000000000 ) ) ;
#5454 = FACE_OUTER_BOUND ( 'NONE', #3509, .T. ) ;
#5455 = ORIENTED_EDGE ( 'NONE', *, *, #980, .F. ) ;
#5456 = EDGE_CURVE ( 'NONE', #823, #2013, #4600, .T. ) ;
#5457 = CARTESIAN_POINT ( 'NONE',  ( 14.35983982790937219, 17.97565917864960738, 2.741545323018244940 ) ) ;
#5458 = CARTESIAN_POINT ( 'NONE',  ( 13.41482486054668399, 26.39531364385071655, 5.999999999999990230 ) ) ;
#5459 = CARTESIAN_POINT ( 'NONE',  ( -4.238929854785999041, 22.60676047400609789, 37.96628288490439473 ) ) ;
#5460 = DIRECTION ( 'NONE',  ( 1.000000000000000000, 0.000000000000000000, -0.000000000000000000 ) ) ;
#5461 = LINE ( 'NONE', #2009, #4289 ) ;
#5462 = DIRECTION ( 'NONE',  ( 0.000000000000000000, -1.000000000000000000, 0.000000000000000000 ) ) ;
#5463 = VECTOR ( 'NONE', #1509, 1000.000000000000000 ) ;
#5464 = ORIENTED_EDGE ( 'NONE', *, *, #1194, .F. ) ;
#5465 = ORIENTED_EDGE ( 'NONE', *, *, #1323, .T. ) ;
#5466 = VECTOR ( 'NONE', #2431, 1000.000000000000000 ) ;
#5467 = EDGE_CURVE ( 'NONE', #775, #6017, #5399, .T. ) ;
#5468 = CARTESIAN_POINT ( 'NONE',  ( -0.2052511266214760433, -21.25619793154163517, -115.0000000000000000 ) ) ;
#5469 = CARTESIAN_POINT ( 'NONE',  ( -7.443729366988918004E-21, 23.00000000000000000, 24.27501000028010125 ) ) ;
#5470 = CARTESIAN_POINT ( 'NONE',  ( 1.764366888834146385, -24.94145795391612452, 9.917654830493175311 ) ) ;
#5471 = ORIENTED_EDGE ( 'NONE', *, *, #4268, .T. ) ;
#5472 =( REPRESENTATION_RELATIONSHIP ('NONE','NONE', #632, #5606 ) REPRESENTATION_RELATIONSHIP_WITH_TRANSFORMATION ( #5529 )SHAPE_REPRESENTATION_RELATIONSHIP( ) );
#5473 = AXIS2_PLACEMENT_3D ( 'NONE', #6059, #2454, #1694 ) ;
#5474 = DIRECTION ( 'NONE',  ( 7.018670225029080348E-17, -1.000000000000000000, 1.271205363195804239E-14 ) ) ;
#5475 = DIRECTION ( 'NONE',  ( 1.000000000000000000, 0.000000000000000000, 0.000000000000000000 ) ) ;
#5476 = FACE_OUTER_BOUND ( 'NONE', #19, .T. ) ;
#5477 = ORIENTED_EDGE ( 'NONE', *, *, #5355, .T. ) ;
#5478 = DIRECTION ( 'NONE',  ( -1.000000000000000000, -1.852483853906148286E-16, 0.000000000000000000 ) ) ;
#5479 = FACE_OUTER_BOUND ( 'NONE', #2116, .T. ) ;
#5480 = DIRECTION ( 'NONE',  ( 0.000000000000000000, 0.000000000000000000, -1.000000000000000000 ) ) ;
#5481 = CARTESIAN_POINT ( 'NONE',  ( -15.99408614349810698, 25.00000000000000000, -4.336808689942017736E-15 ) ) ;
#5482 = ORIENTED_EDGE ( 'NONE', *, *, #3262, .F. ) ;
#5483 = DIRECTION ( 'NONE',  ( 0.000000000000000000, 0.000000000000000000, 1.000000000000000000 ) ) ;
#5484 = DIRECTION ( 'NONE',  ( -0.000000000000000000, -0.000000000000000000, -1.000000000000000000 ) ) ;
#5485 = CARTESIAN_POINT ( 'NONE',  ( 5.266685217916866613, 22.38944685319058436, 26.43066030061579141 ) ) ;
#5486 = CARTESIAN_POINT ( 'NONE',  ( 17.05141243254545458, -2.957948544529944430E-14, 0.000000000000000000 ) ) ;
#5487 = CARTESIAN_POINT ( 'NONE',  ( 0.000000000000000000, 0.000000000000000000, 23.77500997278103512 ) ) ;
#5488 = ORIENTED_EDGE ( 'NONE', *, *, #5315, .T. ) ;
#5489 = EDGE_LOOP ( 'NONE', ( #342, #3793, #5584, #1193 ) ) ;
#5490 = ORIENTED_EDGE ( 'NONE', *, *, #6019, .T. ) ;
#5491 = VERTEX_POINT ( 'NONE', #49 ) ;
#5492 = DIRECTION ( 'NONE',  ( 0.000000000000000000, 1.740526192617802767E-17, -1.000000000000000000 ) ) ;
#5493 = FACE_OUTER_BOUND ( 'NONE', #4219, .T. ) ;
#5494 = CARTESIAN_POINT ( 'NONE',  ( 8.000000000000000000, 110.3953136438507130, 12.00000000000000000 ) ) ;
#5495 = LINE ( 'NONE', #5047, #5646 ) ;
#5496 = ORIENTED_EDGE ( 'NONE', *, *, #4553, .T. ) ;
#5497 = ADVANCED_FACE ( 'NONE', ( #5887 ), #507, .T. ) ;
#5498 = DIRECTION ( 'NONE',  ( 4.267800136491145533E-16, 1.792884867942127993E-23, 1.000000000000000000 ) ) ;
#5499 = CARTESIAN_POINT ( 'NONE',  ( -2.012341796004660122, -22.91179784512888773, 39.00000000000001421 ) ) ;
#5500 = ADVANCED_FACE ( 'NONE', ( #4511, #5373 ), #1982, .T. ) ;
#5501 = CARTESIAN_POINT ( 'NONE',  ( 8.000000000000021316, 1.481987083124922376E-15, 12.00000000000000000 ) ) ;
#5502 = ORIENTED_EDGE ( 'NONE', *, *, #5024, .T. ) ;
#5503 = ORIENTED_EDGE ( 'NONE', *, *, #4201, .F. ) ;
#5504 = EDGE_CURVE ( 'NONE', #1044, #4562, #5461, .T. ) ;
#5505 = EDGE_CURVE ( 'NONE', #5377, #2461, #1042, .T. ) ;
#5506 = DIRECTION ( 'NONE',  ( 1.000000000000000000, 0.000000000000000000, -0.000000000000000000 ) ) ;
#5507 = CARTESIAN_POINT ( 'NONE',  ( 0.000000000000000000, 120.0000000000000000, 16.00000000000000000 ) ) ;
#5508 = SPHERICAL_SURFACE ( 'NONE', #4311, 40.00000002749906258 ) ;
#5509 = VERTEX_POINT ( 'NONE', #467 ) ;
#5510 = CARTESIAN_POINT ( 'NONE',  ( -3.061616997868383043E-15, -25.00000000000000000, -95.00000000000000000 ) ) ;
#5511 = DIRECTION ( 'NONE',  ( 0.000000000000000000, 0.000000000000000000, -1.000000000000000000 ) ) ;
#5512 = CARTESIAN_POINT ( 'NONE',  ( 7.502604696612909407, 21.74191879359210944, 31.88172732429694989 ) ) ;
#5513 = DIRECTION ( 'NONE',  ( 0.000000000000000000, 0.000000000000000000, -1.000000000000000000 ) ) ;
#5514 = CARTESIAN_POINT ( 'NONE',  ( -8.000000000000000000, 110.3953136438507130, 12.00000000000000000 ) ) ;
#5515 = ORIENTED_EDGE ( 'NONE', *, *, #3538, .T. ) ;
#5516 = ORIENTED_EDGE ( 'NONE', *, *, #3736, .T. ) ;
#5517 = VECTOR ( 'NONE', #84, 1000.000000000000000 ) ;
#5518 = EDGE_LOOP ( 'NONE', ( #6137, #57, #4948, #194 ) ) ;
#5519 = DIRECTION ( 'NONE',  ( -1.000000000000000000, 0.000000000000000000, 0.000000000000000000 ) ) ;
#5520 = AXIS2_PLACEMENT_3D ( 'NONE', #1150, #3117, #5060 ) ;
#5521 = CARTESIAN_POINT ( 'NONE',  ( -16.00000000000000355, 0.000000000000000000, -4.000000000000000000 ) ) ;
#5522 = CARTESIAN_POINT ( 'NONE',  ( 6.500000000000005329, 120.0000000000000000, -4.000000000000000000 ) ) ;
#5523 = DIRECTION ( 'NONE',  ( 1.000000000000000000, 0.000000000000000000, 0.000000000000000000 ) ) ;
#5524 =( GEOMETRIC_REPRESENTATION_CONTEXT ( 3 ) GLOBAL_UNCERTAINTY_ASSIGNED_CONTEXT ( ( #4168 ) ) GLOBAL_UNIT_ASSIGNED_CONTEXT ( ( #1280, #2754, #6118 ) ) REPRESENTATION_CONTEXT ( 'NONE', 'WORKASPACE' ) );
#5525 = DIRECTION ( 'NONE',  ( 1.000000000000000000, 0.000000000000000000, 0.000000000000000000 ) ) ;
#5526 = VERTEX_POINT ( 'NONE', #3008 ) ;
#5527 = EDGE_CURVE ( 'NONE', #2807, #1433, #4390, .T. ) ;
#5528 = PRODUCT_DEFINITION_CONTEXT ( 'detailed design', #1178, 'design' ) ;
#5529 = ITEM_DEFINED_TRANSFORMATION ( 'NONE', 'NONE', #184,  #6349 ) ;
#5530 = CIRCLE ( 'NONE', #5750, 19.00000000000000000 ) ;
#5531 = APPLICATION_PROTOCOL_DEFINITION ( 'draft international standard', 'automotive_design', 1998, #5893 ) ;
#5532 = DIRECTION ( 'NONE',  ( -0.000000000000000000, 0.000000000000000000, 1.000000000000000000 ) ) ;
#5533 = EDGE_CURVE ( 'NONE', #4831, #5346, #4706, .T. ) ;
#5534 = ORIENTED_EDGE ( 'NONE', *, *, #4603, .F. ) ;
#5535 = DIRECTION ( 'NONE',  ( 1.000000000000000000, 0.000000000000000000, 0.000000000000000000 ) ) ;
#5536 = VERTEX_POINT ( 'NONE', #1526 ) ;
#5537 = AXIS2_PLACEMENT_3D ( 'NONE', #278, #1882, #2746 ) ;
#5538 = CARTESIAN_POINT ( 'NONE',  ( -3.061616997868383043E-15, -25.00000000000000000, -95.00000000000000000 ) ) ;
#5539 = ADVANCED_FACE ( 'NONE', ( #3519 ), #4943, .F. ) ;
#5540 = CARTESIAN_POINT ( 'NONE',  ( 0.2052511266213299934, 21.25619793154162807, -45.00000000000000000 ) ) ;
#5541 = EDGE_CURVE ( 'NONE', #4432, #5958, #4026, .T. ) ;
#5542 = DIRECTION ( 'NONE',  ( 0.000000000000000000, 0.000000000000000000, 1.000000000000000000 ) ) ;
#5543 = EDGE_LOOP ( 'NONE', ( #5673, #2846 ) ) ;
#5544 = CARTESIAN_POINT ( 'NONE',  ( -15.63674378938990905, 16.87422613917172143, 0.7336288283346519279 ) ) ;
#5545 = AXIS2_PLACEMENT_3D ( 'NONE', #6045, #734, #4155 ) ;
#5546 = DIRECTION ( 'NONE',  ( -0.000000000000000000, -0.000000000000000000, -1.000000000000000000 ) ) ;
#5547 = CARTESIAN_POINT ( 'NONE',  ( 4.599867106623924506, 22.53795783706889821, 25.83444357079220666 ) ) ;
#5548 = EDGE_CURVE ( 'NONE', #6319, #1301, #4481, .T. ) ;
#5549 = AXIS2_PLACEMENT_3D ( 'NONE', #6269, #3875, #2777 ) ;
#5550 = CARTESIAN_POINT ( 'NONE',  ( 13.04517011400474757, 21.32889776003925064, 4.312637851115578513 ) ) ;
#5551 = CIRCLE ( 'NONE', #3082, 17.00000000000000000 ) ;
#5552 = CARTESIAN_POINT ( 'NONE',  ( -43.99999999999990052, 13.41640786499905147, -160.0000000000000284 ) ) ;
#5553 = ORIENTED_EDGE ( 'NONE', *, *, #4275, .F. ) ;
#5554 = ORIENTED_EDGE ( 'NONE', *, *, #1731, .F. ) ;
#5555 = ORIENTED_EDGE ( 'NONE', *, *, #6292, .F. ) ;
#5556 = VERTEX_POINT ( 'NONE', #6005 ) ;
#5557 = CIRCLE ( 'NONE', #4940, 6.500000000000000000 ) ;
#5558 = DIRECTION ( 'NONE',  ( 0.000000000000000000, 0.000000000000000000, -1.000000000000000000 ) ) ;
#5559 = EDGE_CURVE ( 'NONE', #768, #5017, #2455, .T. ) ;
#5560 = CARTESIAN_POINT ( 'NONE',  ( 262.0000000000000000, 68.99999999999997158, 110.0000000000000000 ) ) ;
#5561 = CARTESIAN_POINT ( 'NONE',  ( 7.947562104483774093, 68.75545066608756883, 12.00000000000000000 ) ) ;
#5562 = AXIS2_PLACEMENT_3D ( 'NONE', #3566, #3113, #5089 ) ;
#5563 = CARTESIAN_POINT ( 'NONE',  ( 16.23652742703164975, 37.28747423195200383, -195.0000000000000000 ) ) ;
#5564 = DIRECTION ( 'NONE',  ( -1.000000000000000000, 0.000000000000000000, 0.000000000000000000 ) ) ;
#5565 = ORIENTED_EDGE ( 'NONE', *, *, #2197, .T. ) ;
#5566 = PRODUCT_CONTEXT ( 'NONE', #1590, 'mechanical' ) ;
#5567 = LINE ( 'NONE', #1724, #3454 ) ;
#5568 = VECTOR ( 'NONE', #4464, 1000.000000000000000 ) ;
#5569 = CIRCLE ( 'NONE', #3815, 46.00000000000000000 ) ;
#5570 = VERTEX_POINT ( 'NONE', #4455 ) ;
#5571 = DIRECTION ( 'NONE',  ( 1.000000000000000000, 0.000000000000000000, 0.000000000000000000 ) ) ;
#5572 = EDGE_LOOP ( 'NONE', ( #1726, #3867, #2176, #5980 ) ) ;
#5573 = VECTOR ( 'NONE', #2150, 1000.000000000000000 ) ;
#5574 = CARTESIAN_POINT ( 'NONE',  ( 44.64065620456912598, 28.99954194078667413, -130.0000000000000000 ) ) ;
#5575 = CARTESIAN_POINT ( 'NONE',  ( 0.000000000000000000, 0.000000000000000000, 0.000000000000000000 ) ) ;
#5576 = CYLINDRICAL_SURFACE ( 'NONE', #5840, 17.00000000000000000 ) ;
#5577 = PLANE ( 'NONE',  #2985 ) ;
#5578 = ORIENTED_EDGE ( 'NONE', *, *, #6105, .T. ) ;
#5579 = CARTESIAN_POINT ( 'NONE',  ( -3.009099790203600300, 22.80648947684007410, 9.749155414846011780 ) ) ;
#5580 = CARTESIAN_POINT ( 'NONE',  ( 44.00000000000000000, -13.41640786499874771, 0.000000000000000000 ) ) ;
#5581 = CARTESIAN_POINT ( 'NONE',  ( -7.059265739357024394, 21.89000174688035827, 29.23188816227238362 ) ) ;
#5582 = CARTESIAN_POINT ( 'NONE',  ( -15.23040061807463630, 19.83277885499231630, 1.438641001509332717 ) ) ;
#5583 = CARTESIAN_POINT ( 'NONE',  ( 4.238929854785999041, -22.60676047400609789, 37.96628288490439473 ) ) ;
#5584 = ORIENTED_EDGE ( 'NONE', *, *, #3324, .F. ) ;
#5585 = ORIENTED_EDGE ( 'NONE', *, *, #3601, .T. ) ;
#5586 = CARTESIAN_POINT ( 'NONE',  ( 0.000000000000000000, 0.000000000000000000, 0.000000000000000000 ) ) ;
#5587 = ADVANCED_FACE ( 'NONE', ( #1468 ), #2937, .F. ) ;
#5588 = AXIS2_PLACEMENT_3D ( 'NONE', #4385, #5815, #1428 ) ;
#5589 = CARTESIAN_POINT ( 'NONE',  ( 0.000000000000000000, 0.000000000000000000, 41.00000000000000000 ) ) ;
#5590 = DIRECTION ( 'NONE',  ( -0.000000000000000000, -0.000000000000000000, -1.000000000000000000 ) ) ;
#5591 = DIRECTION ( 'NONE',  ( -0.000000000000000000, 0.000000000000000000, -1.000000000000000000 ) ) ;
#5592 = CARTESIAN_POINT ( 'NONE',  ( 12.50000000000001421, 120.0000000000000000, 16.00000000000000000 ) ) ;
#5593 = EDGE_LOOP ( 'NONE', ( #5402, #1175, #380, #3119, #3011, #4655, #4457 ) ) ;
#5594 = DIRECTION ( 'NONE',  ( -1.000000000000000000, -0.000000000000000000, -0.000000000000000000 ) ) ;
#5595 = CARTESIAN_POINT ( 'NONE',  ( 64.99991398172927859, 76.99999716619419132, 281.0000000000000000 ) ) ;
#5596 = VERTEX_POINT ( 'NONE', #3189 ) ;
#5597 = PRODUCT_DEFINITION_SHAPE ( 'NONE', 'NONE',  #6366 ) ;
#5598 = LINE ( 'NONE', #4015, #5045 ) ;
#5599 = ORIENTED_EDGE ( 'NONE', *, *, #5147, .F. ) ;
#5600 = FACE_OUTER_BOUND ( 'NONE', #3039, .T. ) ;
#5601 = DIRECTION ( 'NONE',  ( 0.000000000000000000, -1.740526192617802767E-17, -1.000000000000000000 ) ) ;
#5602 = CARTESIAN_POINT ( 'NONE',  ( 44.00000000000000000, -13.41640786499873705, -30.00000000000000000 ) ) ;
#5603 = CARTESIAN_POINT ( 'NONE',  ( 18.00000000000000355, 100.3953136438507272, 10.00000000000000000 ) ) ;
#5604 = CARTESIAN_POINT ( 'NONE',  ( -43.99999999999987921, 13.41640786499904969, -115.0000000000000000 ) ) ;
#5605 = ORIENTED_EDGE ( 'NONE', *, *, #3074, .F. ) ;
#5606 = SHAPE_REPRESENTATION ( 'Part 32,6_Varsay\X2\0131\X0\lan', ( #6349 ), #1412 ) ;
#5607 = LINE ( 'NONE', #1673, #5156 ) ;
#5608 = CARTESIAN_POINT ( 'NONE',  ( -4.600626795032661143, 22.53777557106161922, 25.83521031145350122 ) ) ;
#5609 = CARTESIAN_POINT ( 'NONE',  ( -0.8953912278517158763, 24.98774879684974692, 9.982794782258025634 ) ) ;
#5610 = DIRECTION ( 'NONE',  ( -0.000000000000000000, -0.000000000000000000, -1.000000000000000000 ) ) ;
#5611 = EDGE_LOOP ( 'NONE', ( #2165, #2959, #2994, #5891 ) ) ;
#5612 = CIRCLE ( 'NONE', #682, 24.99999999999999289 ) ;
#5613 = VERTEX_POINT ( 'NONE', #1648 ) ;
#5614 = EDGE_CURVE ( 'NONE', #4645, #1019, #1159, .T. ) ;
#5615 = AXIS2_PLACEMENT_3D ( 'NONE', #646, #1566, #675 ) ;
#5616 = VERTEX_POINT ( 'NONE', #3549 ) ;
#5617 = FACE_OUTER_BOUND ( 'NONE', #848, .T. ) ;
#5618 = EDGE_CURVE ( 'NONE', #5570, #1679, #2131, .T. ) ;
#5619 = DIRECTION ( 'NONE',  ( -0.000000000000000000, -0.000000000000000000, -1.000000000000000000 ) ) ;
#5620 = B_SPLINE_CURVE_WITH_KNOTS ( 'NONE', 3,
 ( #5662, #223, #1243, #6111, #5631, #6212, #3205, #3172, #1275, #5211, #3761, #5151, #804, #2749, #2173, #3731, #5693, #323, #5728, #2273, #5183, #1304, #3273, #4130, #5247, #352, #3236, #6181, #3654, #835, #2786, #2714, #4689, #283, #741, #2687, #2205, #2236, #4161, #1764, #6140, #3526 ),
 .UNSPECIFIED., .F., .F.,
 ( 4, 2, 2, 2, 2, 2, 2, 2, 2, 2, 2, 2, 2, 2, 2, 2, 2, 2, 2, 2, 4 ),
 ( 0.000000000000000000, 0.002617858692138167777, 0.005235717384276335554, 0.006544646730345418141, 0.007853576076414500728, 0.01047143476855266243, 0.01308929346069082240, 0.01439822280675990239, 0.01570715215282898758, 0.01832501084496714408, 0.01963394019103622407, 0.02094286953710530058, 0.02356072822924346055, 0.02486965757531254054, 0.02617858692138162399, 0.02879644561351977702, 0.03141430430565794046, 0.03403216299779609350, 0.03665002168993425347, 0.03926788038207241344, 0.04188573907421057341 ),
 .UNSPECIFIED. ) ;
#5621 = DIRECTION ( 'NONE',  ( 1.000000000000000000, 0.000000000000000000, 0.000000000000000000 ) ) ;
#5622 = DIRECTION ( 'NONE',  ( 1.000000000000000000, 0.000000000000000000, 0.000000000000000000 ) ) ;
#5623 = VECTOR ( 'NONE', #887, 1000.000000000000000 ) ;
#5624 = AXIS2_PLACEMENT_3D ( 'NONE', #2177, #2664, #6185 ) ;
#5625 = EDGE_CURVE ( 'NONE', #2831, #1433, #4147, .T. ) ;
#5626 = DIRECTION ( 'NONE',  ( 0.000000000000000000, 0.000000000000000000, -1.000000000000000000 ) ) ;
#5627 = ORIENTED_EDGE ( 'NONE', *, *, #2548, .F. ) ;
#5628 = AXIS2_PLACEMENT_3D ( 'NONE', #5998, #4043, #3057 ) ;
#5629 = EDGE_CURVE ( 'NONE', #4881, #3333, #2593, .T. ) ;
#5630 = PRODUCT_CONTEXT ( 'NONE', #4351, 'mechanical' ) ;
#5631 = CARTESIAN_POINT ( 'NONE',  ( -13.87989846901268187, -18.35105360579683165, 3.366461006762181185 ) ) ;
#5632 = VERTEX_POINT ( 'NONE', #5170 ) ;
#5633 = CYLINDRICAL_SURFACE ( 'NONE', #2158, 25.00000000000000000 ) ;
#5634 = ORIENTED_EDGE ( 'NONE', *, *, #5738, .T. ) ;
#5635 = ADVANCED_FACE ( 'NONE', ( #6260, #6231 ), #5326, .F. ) ;
#5636 = CIRCLE ( 'NONE', #3268, 46.00000000000000000 ) ;
#5637 = LINE ( 'NONE', #4765, #1601 ) ;
#5638 = CYLINDRICAL_SURFACE ( 'NONE', #129, 12.50000000000000355 ) ;
#5639 = CARTESIAN_POINT ( 'NONE',  ( -3.081487911019577365E-30, 5.660601460262082306E-46, 281.0000000000000000 ) ) ;
#5640 = AXIS2_PLACEMENT_3D ( 'NONE', #4839, #2386, #4346 ) ;
#5641 = LINE ( 'NONE', #5604, #2871 ) ;
#5642 = VERTEX_POINT ( 'NONE', #5267 ) ;
#5643 = CARTESIAN_POINT ( 'NONE',  ( -4.293665609699220731, 22.59978795717626454, 9.479591363866271436 ) ) ;
#5644 = CARTESIAN_POINT ( 'NONE',  ( 0.000000000000000000, 0.000000000000000000, 12.00000000000000000 ) ) ;
#5645 = DIRECTION ( 'NONE',  ( 0.000000000000000000, -1.000000000000000000, 0.000000000000000000 ) ) ;
#5646 = VECTOR ( 'NONE', #2107, 1000.000000000000000 ) ;
#5647 = CARTESIAN_POINT ( 'NONE',  ( 12.19460461707454968, 21.82662405552712315, 5.169298567843264358 ) ) ;
#5648 = CARTESIAN_POINT ( 'NONE',  ( 6.980300741495532257, -21.91538084489497962, 34.52732716285097325 ) ) ;
#5649 = VERTEX_POINT ( 'NONE', #787 ) ;
#5650 = AXIS2_PLACEMENT_3D ( 'NONE', #5674, #4115, #1699 ) ;
#5651 = VERTEX_POINT ( 'NONE', #882 ) ;
#5652 = CARTESIAN_POINT ( 'NONE',  ( -0.9837646592764054398, 24.98184996318331130, 39.21432222910941334 ) ) ;
#5653 = AXIS2_PLACEMENT_3D ( 'NONE', #2650, #244, #275 ) ;
#5654 = CIRCLE ( 'NONE', #4512, 22.67164836619068424 ) ;
#5655 = CARTESIAN_POINT ( 'NONE',  ( 44.00000000000009948, 13.41640786499835514, -130.0000000000000000 ) ) ;
#5656 = AXIS2_PLACEMENT_3D ( 'NONE', #4624, #2654, #3653 ) ;
#5657 = CARTESIAN_POINT ( 'NONE',  ( 0.000000000000000000, 0.000000000000000000, 281.0000000000000000 ) ) ;
#5658 = DIRECTION ( 'NONE',  ( -1.000000000000000000, 0.000000000000000000, 0.000000000000000000 ) ) ;
#5659 = VERTEX_POINT ( 'NONE', #2804 ) ;
#5660 = CARTESIAN_POINT ( 'NONE',  ( 0.000000000000000000, 0.000000000000000000, 41.00000000000000000 ) ) ;
#5661 = VERTEX_POINT ( 'NONE', #1879 ) ;
#5662 = CARTESIAN_POINT ( 'NONE',  ( -15.99408614349810698, -16.52843635781563592, 0.000000000000000000 ) ) ;
#5663 = ORIENTED_EDGE ( 'NONE', *, *, #3056, .T. ) ;
#5664 = DIRECTION ( 'NONE',  ( 0.000000000000000000, 0.000000000000000000, 1.000000000000000000 ) ) ;
#5665 = EDGE_LOOP ( 'NONE', ( #5233, #581, #2793, #6306 ) ) ;
#5666 = DIRECTION ( 'NONE',  ( -0.000000000000000000, 0.000000000000000000, -1.000000000000000000 ) ) ;
#5667 = CIRCLE ( 'NONE', #2782, 22.67164836619067714 ) ;
#5668 = UNCERTAINTY_MEASURE_WITH_UNIT (LENGTH_MEASURE( 1.000000000000000082E-05 ), #3147, 'distance_accuracy_value', 'NONE');
#5669 = CARTESIAN_POINT ( 'NONE',  ( 22.00000000000000000, 2.694222958124176809E-15, 41.00000000000000000 ) ) ;
#5670 = DIRECTION ( 'NONE',  ( -0.000000000000000000, -0.000000000000000000, -1.000000000000000000 ) ) ;
#5671 = PRODUCT_DEFINITION_CONTEXT ( 'detailed design', #2379, 'design' ) ;
#5672 = CARTESIAN_POINT ( 'NONE',  ( -2.432532833620815182, -24.88553977760506797, 24.66355118963700122 ) ) ;
#5673 = ORIENTED_EDGE ( 'NONE', *, *, #2577, .T. ) ;
#5674 = CARTESIAN_POINT ( 'NONE',  ( 42.00000000000000000, 69.00000000000000000, 0.000000000000000000 ) ) ;
#5675 = ORIENTED_EDGE ( 'NONE', *, *, #2081, .T. ) ;
#5676 = CYLINDRICAL_SURFACE ( 'NONE', #1350, 7.500000000000000000 ) ;
#5677 = CARTESIAN_POINT ( 'NONE',  ( -44.00000000000000000, -13.41640786499873350, -180.0000000000000000 ) ) ;
#5678 = VECTOR ( 'NONE', #3664, 1000.000000000000000 ) ;
#5679 = FACE_BOUND ( 'NONE', #4244, .T. ) ;
#5680 = CARTESIAN_POINT ( 'NONE',  ( 4.782950468712823699, -22.50022147858462418, 37.56939778472803226 ) ) ;
#5681 = ORIENTED_EDGE ( 'NONE', *, *, #4871, .T. ) ;
#5682 = VERTEX_POINT ( 'NONE', #4774 ) ;
#5683 = DIRECTION ( 'NONE',  ( -1.000000000000000000, 0.000000000000000000, 0.000000000000000000 ) ) ;
#5684 = LINE ( 'NONE', #6132, #276 ) ;
#5685 = LINE ( 'NONE', #2134, #99 ) ;
#5686 = DIRECTION ( 'NONE',  ( -0.000000000000000000, -0.000000000000000000, -1.000000000000000000 ) ) ;
#5687 = ORIENTED_EDGE ( 'NONE', *, *, #5015, .T. ) ;
#5688 = CARTESIAN_POINT ( 'NONE',  ( -3.081487911019577365E-30, 5.660601460262082306E-46, 0.000000000000000000 ) ) ;
#5689 = ORIENTED_EDGE ( 'NONE', *, *, #5363, .F. ) ;
#5690 = AXIS2_PLACEMENT_3D ( 'NONE', #1011, #1390, #3351 ) ;
#5691 = CARTESIAN_POINT ( 'NONE',  ( 0.000000000000000000, -24.25762350764758679, 12.00000000000000000 ) ) ;
#5692 = ITEM_DEFINED_TRANSFORMATION ( 'NONE', 'NONE', #698,  #6349 ) ;
#5693 = CARTESIAN_POINT ( 'NONE',  ( -5.608440128082920140, -22.30969483029271672, 9.098285821462422263 ) ) ;
#5694 = ORIENTED_EDGE ( 'NONE', *, *, #3898, .F. ) ;
#5695 = DIRECTION ( 'NONE',  ( -0.000000000000000000, -0.000000000000000000, -1.000000000000000000 ) ) ;
#5696 = ORIENTED_EDGE ( 'NONE', *, *, #6292, .T. ) ;
#5697 = EDGE_CURVE ( 'NONE', #4562, #2452, #5530, .T. ) ;
#5698 = EDGE_CURVE ( 'NONE', #1574, #4961, #4249, .T. ) ;
#5699 = CARTESIAN_POINT ( 'NONE',  ( 279.0000000000000000, 68.99999999999997158, 110.0000000000000000 ) ) ;
#5700 = ADVANCED_FACE ( 'NONE', ( #5679, #2288 ), #5712, .F. ) ;
#5701 = CARTESIAN_POINT ( 'NONE',  ( -17.00000000000000000, 25.00000000000000355, 0.000000000000000000 ) ) ;
#5702 = DIRECTION ( 'NONE',  ( -1.000000000000000000, 0.000000000000000000, 0.000000000000000000 ) ) ;
#5703 = CARTESIAN_POINT ( 'NONE',  ( -7.500037790182080499, -23.84846815096123507, 31.28125562555191763 ) ) ;
#5704 = ORIENTED_EDGE ( 'NONE', *, *, #3218, .F. ) ;
#5705 = EDGE_CURVE ( 'NONE', #4530, #12, #5850, .T. ) ;
#5706 = EDGE_CURVE ( 'NONE', #3426, #1557, #1516, .T. ) ;
#5707 = PRODUCT_DEFINITION_CONTEXT ( 'detailed design', #4808, 'design' ) ;
#5708 = ORIENTED_EDGE ( 'NONE', *, *, #4564, .F. ) ;
#5709 = VERTEX_POINT ( 'NONE', #6197 ) ;
#5710 = DIRECTION ( 'NONE',  ( -0.000000000000000000, -0.000000000000000000, 1.000000000000000000 ) ) ;
#5711 = CARTESIAN_POINT ( 'NONE',  ( -17.00000000000000000, 25.00000000000000355, -30.00000000000000000 ) ) ;
#5712 = PLANE ( 'NONE',  #83 ) ;
#5713 = CARTESIAN_POINT ( 'NONE',  ( 3.063555513103408678, -22.79893987554409662, 24.91467890029023025 ) ) ;
#5714 = ORIENTED_EDGE ( 'NONE', *, *, #5169, .F. ) ;
#5715 = EDGE_CURVE ( 'NONE', #1906, #2036, #3346, .T. ) ;
#5716 = EDGE_CURVE ( 'NONE', #981, #2906, #1777, .T. ) ;
#5717 = ORIENTED_EDGE ( 'NONE', *, *, #517, .T. ) ;
#5718 = CARTESIAN_POINT ( 'NONE',  ( -0.2456693407522352601, 24.99999999999999645, 39.27501000028010480 ) ) ;
#5719 = CARTESIAN_POINT ( 'NONE',  ( 0.000000000000000000, 0.000000000000000000, 1.734723475976807094E-15 ) ) ;
#5720 = DIRECTION ( 'NONE',  ( 1.000000000000000000, 0.000000000000000000, 0.000000000000000000 ) ) ;
#5721 = AXIS2_PLACEMENT_3D ( 'NONE', #5020, #2569, #1032 ) ;
#5722 = DIRECTION ( 'NONE',  ( 1.000000000000000000, 0.000000000000000000, 0.000000000000000000 ) ) ;
#5723 = AXIS2_PLACEMENT_3D ( 'NONE', #2132, #3555, #1098 ) ;
#5724 = VERTEX_POINT ( 'NONE', #4707 ) ;
#5725 = ORIENTED_EDGE ( 'NONE', *, *, #3533, .T. ) ;
#5726 = CARTESIAN_POINT ( 'NONE',  ( 0.000000000000000000, 76.99999716619419132, 276.0000000000000000 ) ) ;
#5727 = ITEM_DEFINED_TRANSFORMATION ( 'NONE', 'NONE', #4282,  #6349 ) ;
#5728 = CARTESIAN_POINT ( 'NONE',  ( -3.536994606882255532, -22.74309932279132340, 9.666805580179055113 ) ) ;
#5729 = CIRCLE ( 'NONE', #1506, 20.00000000000000000 ) ;
#5730 = CARTESIAN_POINT ( 'NONE',  ( -12.89883946988004304, 28.41146683342871171, 9.483046795230265502 ) ) ;
#5731 = EDGE_LOOP ( 'NONE', ( #3141, #2334, #5414, #2099, #2980, #1867, #5207, #4992, #1497, #4851, #1967, #3424, #2808, #2620 ) ) ;
#5732 = ADVANCED_FACE ( 'NONE', ( #3839 ), #1360, .F. ) ;
#5733 = DIRECTION ( 'NONE',  ( -3.903561672282191229E-16, 1.000000000000000000, -0.000000000000000000 ) ) ;
#5734 = VERTEX_POINT ( 'NONE', #3749 ) ;
#5735 = ORIENTED_EDGE ( 'NONE', *, *, #2856, .T. ) ;
#5736 = CIRCLE ( 'NONE', #5327, 45.99999999999997868 ) ;
#5737 = ADVANCED_FACE ( 'NONE', ( #3779, #3316 ), #5296, .T. ) ;
#5738 = EDGE_CURVE ( 'NONE', #1816, #3396, #5440, .T. ) ;
#5739 = DIRECTION ( 'NONE',  ( -0.000000000000000000, 0.000000000000000000, -1.000000000000000000 ) ) ;
#5740 = CARTESIAN_POINT ( 'NONE',  ( 0.000000000000000000, 0.000000000000000000, -160.0000000000000284 ) ) ;
#5741 = CARTESIAN_POINT ( 'NONE',  ( -3.769534566620170057, -24.71760338780762467, 38.27724873576356401 ) ) ;
#5742 = VERTEX_POINT ( 'NONE', #402 ) ;
#5743 = AXIS2_PLACEMENT_3D ( 'NONE', #58, #131, #2085 ) ;
#5744 = CARTESIAN_POINT ( 'NONE',  ( 0.000000000000000000, 0.000000000000000000, 0.000000000000000000 ) ) ;
#5745 = ORIENTED_EDGE ( 'NONE', *, *, #5084, .F. ) ;
#5746 = CARTESIAN_POINT ( 'NONE',  ( 3.122849337825746672E-15, 17.00000000000000000, 301.0000000000000568 ) ) ;
#5747 = CARTESIAN_POINT ( 'NONE',  ( 4.781067518356564072, 22.50057576469317411, 37.57069195157705366 ) ) ;
#5748 = EDGE_CURVE ( 'NONE', #5642, #661, #3157, .T. ) ;
#5749 = EDGE_CURVE ( 'NONE', #4236, #5889, #2355, .T. ) ;
#5750 = AXIS2_PLACEMENT_3D ( 'NONE', #4741, #909, #2731 ) ;
#5751 = CARTESIAN_POINT ( 'NONE',  ( 0.000000000000000000, 0.000000000000000000, -248.0000000000000000 ) ) ;
#5752 = CARTESIAN_POINT ( 'NONE',  ( 6.978968890507021960, -21.91580918028467195, 29.01915572147083822 ) ) ;
#5753 = VERTEX_POINT ( 'NONE', #1384 ) ;
#5754 = CIRCLE ( 'NONE', #4404, 17.00000000000000000 ) ;
#5755 = ORIENTED_EDGE ( 'NONE', *, *, #4072, .T. ) ;
#5756 = EDGE_CURVE ( 'NONE', #258, #5742, #3050, .T. ) ;
#5757 = CARTESIAN_POINT ( 'NONE',  ( -6.506525936991941705, 24.14011651440024764, 28.01231256153109683 ) ) ;
#5758 = CARTESIAN_POINT ( 'NONE',  ( -17.05141243254543681, -12.25762350764760455, 12.00000000000000000 ) ) ;
#5759 = CARTESIAN_POINT ( 'NONE',  ( 0.000000000000000000, 0.000000000000000000, 47.00000000000000711 ) ) ;
#5760 = AXIS2_PLACEMENT_3D ( 'NONE', #6288, #1285, #5324 ) ;
#5761 = DIRECTION ( 'NONE',  ( 1.000000000000000000, 0.000000000000000000, 0.000000000000000000 ) ) ;
#5762 = ORIENTED_EDGE ( 'NONE', *, *, #5237, .T. ) ;
#5763 = ORIENTED_EDGE ( 'NONE', *, *, #5316, .T. ) ;
#5764 = ADVANCED_FACE ( 'NONE', ( #1548 ), #2484, .F. ) ;
#5765 = VECTOR ( 'NONE', #527, 1000.000000000000000 ) ;
#5766 = LINE ( 'NONE', #417, #5985 ) ;
#5767 = DIRECTION ( 'NONE',  ( 0.000000000000000000, 0.000000000000000000, -1.000000000000000000 ) ) ;
#5768 = CIRCLE ( 'NONE', #3803, 19.00000000000000000 ) ;
#5769 = ORIENTED_EDGE ( 'NONE', *, *, #2570, .T. ) ;
#5770 = CARTESIAN_POINT ( 'NONE',  ( -3.122849337825752983E-15, -17.00000000000000000, -20.00000000000000000 ) ) ;
#5771 = EDGE_LOOP ( 'NONE', ( #3240, #4217, #5627, #960 ) ) ;
#5772 = CIRCLE ( 'NONE', #2053, 67.50000000000000000 ) ;
#5773 = CARTESIAN_POINT ( 'NONE',  ( 0.000000000000000000, 0.000000000000000000, 0.000000000000000000 ) ) ;
#5774 = SHAPE_REPRESENTATION_RELATIONSHIP ( 'NONE' , 'NONE' ,  #3711, #4474 ) ;
#5775 = CARTESIAN_POINT ( 'NONE',  ( -44.43364355155666345, 29.42304313293564988, -95.00000000000000000 ) ) ;
#5776 = CARTESIAN_POINT ( 'NONE',  ( -25.00000000000000000, 0.000000000000000000, 47.00000000000000711 ) ) ;
#5777 = AXIS2_PLACEMENT_3D ( 'NONE', #2175, #1081, #712 ) ;
#5778 = CARTESIAN_POINT ( 'NONE',  ( -6.507303803555988253, -24.13991014445888439, 28.01358234833887195 ) ) ;
#5779 = ORIENTED_EDGE ( 'NONE', *, *, #786, .T. ) ;
#5780 = CARTESIAN_POINT ( 'NONE',  ( -16.23652742703189489, -37.28747423195188304, -95.00000000000000000 ) ) ;
#5781 = AXIS2_PLACEMENT_3D ( 'NONE', #4605, #3547, #724 ) ;
#5782 = CARTESIAN_POINT ( 'NONE',  ( 4.956647734651109971, 24.50626513604599310, 37.42488445140202202 ) ) ;
#5783 = DIRECTION ( 'NONE',  ( -1.000000000000000000, 0.000000000000000000, 0.000000000000000000 ) ) ;
#5784 = CARTESIAN_POINT ( 'NONE',  ( -17.00000000000000355, -24.99999999999999645, -95.00000000000000000 ) ) ;
#5785 = CARTESIAN_POINT ( 'NONE',  ( 6.385057176062306716, -22.09706105569707191, 27.81520467947423114 ) ) ;
#5786 = ORIENTED_EDGE ( 'NONE', *, *, #4124, .T. ) ;
#5787 = EDGE_LOOP ( 'NONE', ( #5242, #5223, #3036, #3914 ) ) ;
#5788 = CARTESIAN_POINT ( 'NONE',  ( -5.474672603935806237, 24.39383812260184214, 36.90705202433113641 ) ) ;
#5789 = VECTOR ( 'NONE', #2836, 1000.000000000000000 ) ;
#5790 = LINE ( 'NONE', #6266, #2219 ) ;
#5791 = DIRECTION ( 'NONE',  ( -0.000000000000000000, -0.000000000000000000, -1.000000000000000000 ) ) ;
#5792 = DIRECTION ( 'NONE',  ( -0.000000000000000000, -0.000000000000000000, 1.000000000000000000 ) ) ;
#5793 = ORIENTED_EDGE ( 'NONE', *, *, #499, .F. ) ;
#5794 = VERTEX_POINT ( 'NONE', #4447 ) ;
#5795 = EDGE_CURVE ( 'NONE', #341, #5286, #3279, .T. ) ;
#5796 = EDGE_LOOP ( 'NONE', ( #4945, #6049, #5321, #5396 ) ) ;
#5797 = CYLINDRICAL_SURFACE ( 'NONE', #638, 22.00000000000000000 ) ;
#5798 = CARTESIAN_POINT ( 'NONE',  ( -13.05961095629095503, 27.77190499716703442, 9.030829679283291611 ) ) ;
#5799 = FACE_OUTER_BOUND ( 'NONE', #3394, .T. ) ;
#5800 = VERTEX_POINT ( 'NONE', #1035 ) ;
#5801 = CARTESIAN_POINT ( 'NONE',  ( -1.331801922117356663E-14, -72.49991987048069575, 1.734723475976807094E-15 ) ) ;
#5802 =( NAMED_UNIT ( * ) SI_UNIT ( $, .STERADIAN. ) SOLID_ANGLE_UNIT ( ) );
#5803 = FACE_OUTER_BOUND ( 'NONE', #1787, .T. ) ;
#5804 = FACE_OUTER_BOUND ( 'NONE', #1327, .T. ) ;
#5805 = CARTESIAN_POINT ( 'NONE',  ( -7.438449848406675891, -23.86776331625856429, 32.76532521224502403 ) ) ;
#5806 = EDGE_LOOP ( 'NONE', ( #1570, #567, #830, #4258 ) ) ;
#5807 = FILL_AREA_STYLE ('',( #2318 ) ) ;
#5808 = DIRECTION ( 'NONE',  ( 0.000000000000000000, 0.000000000000000000, 1.000000000000000000 ) ) ;
#5809 = DIRECTION ( 'NONE',  ( -0.000000000000000000, -0.000000000000000000, -1.000000000000000000 ) ) ;
#5810 = CARTESIAN_POINT ( 'NONE',  ( 3.466163672723409750, -22.74070890941651157, 25.10873389944362444 ) ) ;
#5811 = ORIENTED_EDGE ( 'NONE', *, *, #1330, .T. ) ;
#5812 = EDGE_CURVE ( 'NONE', #214, #2898, #2221, .T. ) ;
#5813 = DIRECTION ( 'NONE',  ( 0.000000000000000000, 0.000000000000000000, 1.000000000000000000 ) ) ;
#5814 = ORIENTED_EDGE ( 'NONE', *, *, #483, .F. ) ;
#5815 = DIRECTION ( 'NONE',  ( 1.000000000000000000, -1.836970198721029194E-16, 0.000000000000000000 ) ) ;
#5816 = LINE ( 'NONE', #4290, #5623 ) ;
#5817 = EDGE_CURVE ( 'NONE', #2677, #1781, #67, .T. ) ;
#5818 = LINE ( 'NONE', #6302, #1715 ) ;
#5819 = FACE_OUTER_BOUND ( 'NONE', #5026, .T. ) ;
#5820 = ORIENTED_EDGE ( 'NONE', *, *, #4874, .T. ) ;
#5821 = ORIENTED_EDGE ( 'NONE', *, *, #5015, .F. ) ;
#5822 = EDGE_LOOP ( 'NONE', ( #1002, #1141, #4029, #3447 ) ) ;
#5823 = CARTESIAN_POINT ( 'NONE',  ( 17.05141243254545458, -2.957948544529944430E-14, 12.00000000000000000 ) ) ;
#5824 = CARTESIAN_POINT ( 'NONE',  ( -13.40794989232620615, 26.42147665086397268, 6.529465147186705565 ) ) ;
#5825 = PRODUCT_RELATED_PRODUCT_CATEGORY ( 'part', '', ( #1681 ) ) ;
#5826 = ADVANCED_FACE ( 'NONE', ( #3416 ), #1485, .F. ) ;
#5827 = CIRCLE ( 'NONE', #3038, 166.8359700257217071 ) ;
#5828 = CARTESIAN_POINT ( 'NONE',  ( 8.266016972479206970, -23.60732501453302490, 7.985288904279077116 ) ) ;
#5829 = EDGE_LOOP ( 'NONE', ( #6360, #5118, #3763, #2534 ) ) ;
#5830 = EDGE_CURVE ( 'NONE', #12, #4530, #610, .T. ) ;
#5831 = FACE_OUTER_BOUND ( 'NONE', #3475, .T. ) ;
#5832 = DIRECTION ( 'NONE',  ( 1.000000000000000000, 0.000000000000000000, 0.000000000000000000 ) ) ;
#5833 = EDGE_CURVE ( 'NONE', #427, #5346, #3000, .T. ) ;
#5834 = DIRECTION ( 'NONE',  ( 0.000000000000000000, -1.000000000000000000, -1.247733429937938623E-16 ) ) ;
#5835 = CARTESIAN_POINT ( 'NONE',  ( -15.82602517378898987, 37.28747423195201094, -240.0000000000000000 ) ) ;
#5836 = ORIENTED_EDGE ( 'NONE', *, *, #2936, .F. ) ;
#5837 = EDGE_CURVE ( 'NONE', #3260, #5184, #2924, .T. ) ;
#5838 = AXIS2_PLACEMENT_3D ( 'NONE', #5468, #4057, #6044 ) ;
#5839 = EDGE_CURVE ( 'NONE', #2487, #6022, #4933, .T. ) ;
#5840 = AXIS2_PLACEMENT_3D ( 'NONE', #5160, #2571, #5094 ) ;
#5841 = CARTESIAN_POINT ( 'NONE',  ( 0.000000000000000000, 0.000000000000000000, -273.0000000000000000 ) ) ;
#5842 = LINE ( 'NONE', #1383, #328 ) ;
#5843 = LINE ( 'NONE', #1422, #4167 ) ;
#5844 = VECTOR ( 'NONE', #488, 1000.000000000000000 ) ;
#5845 = CARTESIAN_POINT ( 'NONE',  ( 7.369598735940123824, -21.78745483514939707, 30.31133554494096671 ) ) ;
#5846 = VERTEX_POINT ( 'NONE', #533 ) ;
#5847 = LINE ( 'NONE', #1944, #3576 ) ;
#5848 = CARTESIAN_POINT ( 'NONE',  ( -0.000000000000000000, 134.5953136438507158, 0.000000000000000000 ) ) ;
#5849 = CARTESIAN_POINT ( 'NONE',  ( -6.716176415091607232, 21.99834172012562661, 35.14285310556104491 ) ) ;
#5850 = CIRCLE ( 'NONE', #3059, 25.00000000000000000 ) ;
#5851 = FACE_OUTER_BOUND ( 'NONE', #2216, .T. ) ;
#5852 = PLANE ( 'NONE',  #1309 ) ;
#5853 = CARTESIAN_POINT ( 'NONE',  ( 22.00000000000000000, 2.694222958124176809E-15, 50.00000000000000711 ) ) ;
#5854 = AXIS2_PLACEMENT_3D ( 'NONE', #4035, #127, #642 ) ;
#5855 = AXIS2_PLACEMENT_3D ( 'NONE', #810, #4307, #5319 ) ;
#5856 = VERTEX_POINT ( 'NONE', #2513 ) ;
#5857 = ORIENTED_EDGE ( 'NONE', *, *, #2294, .F. ) ;
#5858 = B_SPLINE_CURVE_WITH_KNOTS ( 'NONE', 3,
 ( #450, #999, #4924, #1413, #4466, #5929, #2851, #4890, #5318, #1377, #4369, #901, #2410, #424, #2376, #4440, #6339, #6316, #1963, #31, #3957, #1508, #3405, #59, #1898, #3857, #3373, #5869, #5385, #967, #1541, #5086, #1629, #578, #3507, #4626, #2055, #4038, #3982, #1080, #2086, #3625, #190, #5499 ),
 .UNSPECIFIED., .F., .F.,
 ( 4, 2, 2, 2, 2, 2, 2, 2, 2, 2, 2, 2, 2, 2, 2, 2, 2, 2, 2, 2, 2, 4 ),
 ( 0.02157941337148385624, 0.02225324431794266020, 0.02292707526440146415, 0.02427473715731907553, 0.02562239905023668690, 0.02697006094315429828, 0.02764389188961310223, 0.02831772283607190271, 0.02966538472898951062, 0.03033921567544831110, 0.03101304662190711506, 0.03236070851482472643, 0.03303453946128352692, 0.03370837040774233434, 0.03505603230065991449, 0.03640369419357750158, 0.03707752514003628125, 0.03775135608649506092, 0.03909901797941260637, 0.04044667987233015183, 0.04179434176524769728, 0.04314200365816523580 ),
 .UNSPECIFIED. ) ;
#5859 = AXIS2_PLACEMENT_3D ( 'NONE', #1544, #5389, #5935 ) ;
#5860 = FACE_OUTER_BOUND ( 'NONE', #5281, .T. ) ;
#5861 = ITEM_DEFINED_TRANSFORMATION ( 'NONE', 'NONE', #3264,  #6349 ) ;
#5862 = CARTESIAN_POINT ( 'NONE',  ( -13.41482486054668044, 26.39531364385071299, 5.999999999999990230 ) ) ;
#5863 = CARTESIAN_POINT ( 'NONE',  ( -7.831318214037678693, -23.74511713421663472, 8.189156644668287299 ) ) ;
#5864 = ORIENTED_EDGE ( 'NONE', *, *, #5437, .F. ) ;
#5865 = VECTOR ( 'NONE', #6169, 1000.000000000000000 ) ;
#5866 = CARTESIAN_POINT ( 'NONE',  ( 0.000000000000000000, 0.000000000000000000, -49.99999999999999289 ) ) ;
#5867 = CIRCLE ( 'NONE', #97, 90.00000000000000000 ) ;
#5868 = CARTESIAN_POINT ( 'NONE',  ( 1.311805171047821572, 63.50744305896921560, 131.1935513772730815 ) ) ;
#5869 = CARTESIAN_POINT ( 'NONE',  ( -7.472848606399997706, -21.75217170649850118, 32.55500807037982725 ) ) ;
#5870 = CIRCLE ( 'NONE', #4726, 6.500000000000005329 ) ;
#5871 = AXIS2_PLACEMENT_3D ( 'NONE', #5148, #2686, #2783 ) ;
#5872 = LINE ( 'NONE', #4891, #6043 ) ;
#5873 = CARTESIAN_POINT ( 'NONE',  ( 0.000000000000000000, -24.25762350764758679, 12.00000000000000000 ) ) ;
#5874 = ORIENTED_EDGE ( 'NONE', *, *, #662, .F. ) ;
#5875 = CYLINDRICAL_SURFACE ( 'NONE', #5244, 25.00000000000000000 ) ;
#5876 = AXIS2_PLACEMENT_3D ( 'NONE', #4574, #3125, #658 ) ;
#5877 = CARTESIAN_POINT ( 'NONE',  ( -4.592425496802576733E-15, -25.00000000000000000, 281.0000000000000000 ) ) ;
#5878 = DIRECTION ( 'NONE',  ( -0.000000000000000000, -0.000000000000000000, -1.000000000000000000 ) ) ;
#5879 = CARTESIAN_POINT ( 'NONE',  ( 16.99999999999999645, -25.00000000000000000, -95.00000000000000000 ) ) ;
#5880 = VERTEX_POINT ( 'NONE', #41 ) ;
#5881 = DIRECTION ( 'NONE',  ( -0.000000000000000000, -0.000000000000000000, 1.000000000000000000 ) ) ;
#5882 = EDGE_LOOP ( 'NONE', ( #1120, #2413, #2266, #4264, #6139, #4134, #3911, #1388, #4806 ) ) ;
#5883 = PLANE ( 'NONE',  #5690 ) ;
#5884 = AXIS2_PLACEMENT_3D ( 'NONE', #5644, #655, #4639 ) ;
#5885 = CIRCLE ( 'NONE', #3975, 17.00000000000000000 ) ;
#5886 = FACE_BOUND ( 'NONE', #5543, .T. ) ;
#5887 = FACE_OUTER_BOUND ( 'NONE', #543, .T. ) ;
#5888 = DIRECTION ( 'NONE',  ( -0.000000000000000000, -0.000000000000000000, -1.000000000000000000 ) ) ;
#5889 = VERTEX_POINT ( 'NONE', #3963 ) ;
#5890 = ORIENTED_EDGE ( 'NONE', *, *, #104, .T. ) ;
#5891 = ORIENTED_EDGE ( 'NONE', *, *, #4581, .T. ) ;
#5892 = CYLINDRICAL_SURFACE ( 'NONE', #1135, 22.00000000000000000 ) ;
#5893 = APPLICATION_CONTEXT ( 'automotive_design' ) ;
#5894 = CYLINDRICAL_SURFACE ( 'NONE', #3695, 17.00000000000000000 ) ;
#5895 = DIRECTION ( 'NONE',  ( 0.000000000000000000, 0.000000000000000000, -1.000000000000000000 ) ) ;
#5896 = VERTEX_POINT ( 'NONE', #5940 ) ;
#5897 = DIRECTION ( 'NONE',  ( 0.000000000000000000, 0.000000000000000000, 1.000000000000000000 ) ) ;
#5898 = CARTESIAN_POINT ( 'NONE',  ( 22.21770253897382474, 3.871672004622519037, -110.0000000000000000 ) ) ;
#5899 = CARTESIAN_POINT ( 'NONE',  ( 17.00000000000000000, 69.00000000000000000, 110.0000000000000000 ) ) ;
#5900 = FACE_OUTER_BOUND ( 'NONE', #3734, .T. ) ;
#5901 = ORIENTED_EDGE ( 'NONE', *, *, #3262, .T. ) ;
#5902 = EDGE_CURVE ( 'NONE', #5846, #3758, #3872, .T. ) ;
#5903 = DIRECTION ( 'NONE',  ( 0.000000000000000000, 0.000000000000000000, -1.000000000000000000 ) ) ;
#5904 = EDGE_CURVE ( 'NONE', #2498, #5491, #3482, .T. ) ;
#5905 = CARTESIAN_POINT ( 'NONE',  ( -6.500000000000006217, 130.6770782520313219, 0.000000000000000000 ) ) ;
#5906 = EDGE_CURVE ( 'NONE', #4140, #5271, #5843, .T. ) ;
#5907 = CARTESIAN_POINT ( 'NONE',  ( 4.953190041214020845, 24.50516424074860922, 26.13799397941501113 ) ) ;
#5908 = EDGE_CURVE ( 'NONE', #760, #4515, #1088, .T. ) ;
#5909 = EDGE_CURVE ( 'NONE', #1953, #2336, #1117, .T. ) ;
#5910 = CARTESIAN_POINT ( 'NONE',  ( -12.66355262481067179, 29.36736923042837333, 2.125736663006382976 ) ) ;
#5911 = LINE ( 'NONE', #1517, #2152 ) ;
#5912 = VERTEX_POINT ( 'NONE', #3150 ) ;
#5913 = CARTESIAN_POINT ( 'NONE',  ( 9.051043717164153790, 21.15747665746626183, 7.546935333285830438 ) ) ;
#5914 = CARTESIAN_POINT ( 'NONE',  ( 13.30659111572998654, 26.80965796039522786, 7.792318603440350877 ) ) ;
#5915 = CYLINDRICAL_SURFACE ( 'NONE', #2395, 166.8359700257217071 ) ;
#5916 = CARTESIAN_POINT ( 'NONE',  ( -3.081487911019577365E-30, 5.660601460262082306E-46, 0.000000000000000000 ) ) ;
#5917 = DIRECTION ( 'NONE',  ( 1.000000000000000000, 0.000000000000000000, -0.000000000000000000 ) ) ;
#5918 = CARTESIAN_POINT ( 'NONE',  ( 44.64065620456912598, 28.99954194078667413, -65.00000000000000000 ) ) ;
#5919 = ORIENTED_EDGE ( 'NONE', *, *, #2734, .F. ) ;
#5920 = EDGE_CURVE ( 'NONE', #3208, #624, #5956, .T. ) ;
#5921 = ORIENTED_EDGE ( 'NONE', *, *, #2271, .F. ) ;
#5922 = ORIENTED_EDGE ( 'NONE', *, *, #1342, .F. ) ;
#5923 = ORIENTED_EDGE ( 'NONE', *, *, #801, .F. ) ;
#5924 = DIRECTION ( 'NONE',  ( -0.000000000000000000, 0.000000000000000000, -1.000000000000000000 ) ) ;
#5925 = DIRECTION ( 'NONE',  ( -1.000000000000000000, 0.000000000000000000, 0.000000000000000000 ) ) ;
#5926 = CARTESIAN_POINT ( 'NONE',  ( 0.000000000000000000, 0.000000000000000000, 41.00000000000000000 ) ) ;
#5927 = ORIENTED_EDGE ( 'NONE', *, *, #3271, .F. ) ;
#5928 = DIRECTION ( 'NONE',  ( -2.225818823798634026E-16, -1.000000000000000222, 0.000000000000000000 ) ) ;
#5929 = CARTESIAN_POINT ( 'NONE',  ( -1.794389728719248733, -22.93422366650650090, 24.47880888172866065 ) ) ;
#5930 = EDGE_CURVE ( 'NONE', #738, #4541, #1923, .T. ) ;
#5931 = DIRECTION ( 'NONE',  ( -1.000000000000000000, -0.000000000000000000, -0.000000000000000000 ) ) ;
#5932 = ORIENTED_EDGE ( 'NONE', *, *, #108, .T. ) ;
#5933 = ORIENTED_EDGE ( 'NONE', *, *, #4637, .T. ) ;
#5934 = AXIS2_PLACEMENT_3D ( 'NONE', #4089, #5492, #1073 ) ;
#5935 = DIRECTION ( 'NONE',  ( -1.000000000000000000, 0.000000000000000000, 0.000000000000000000 ) ) ;
#5936 = FACE_OUTER_BOUND ( 'NONE', #4362, .T. ) ;
#5937 = ADVANCED_FACE ( 'NONE', ( #231 ), #2120, .T. ) ;
#5938 = ADVANCED_FACE ( 'NONE', ( #6061 ), #4532, .T. ) ;
#5939 = AXIS2_PLACEMENT_3D ( 'NONE', #5107, #5238, #2262 ) ;
#5940 = CARTESIAN_POINT ( 'NONE',  ( 8.000000000000003553, 100.3953136438507272, 10.00000000000000000 ) ) ;
#5941 = AXIS2_PLACEMENT_3D ( 'NONE', #5773, #1962, #1409 ) ;
#5942 = PLANE ( 'NONE',  #4832 ) ;
#5943 = ORIENTED_EDGE ( 'NONE', *, *, #2544, .F. ) ;
#5944 = PLANE ( 'NONE',  #2451 ) ;
#5945 = EDGE_CURVE ( 'NONE', #2238, #1244, #3542, .T. ) ;
#5946 = CARTESIAN_POINT ( 'NONE',  ( 13.00740645622773961, 27.97830129128179166, 9.197704556789860320 ) ) ;
#5947 = DIRECTION ( 'NONE',  ( 1.000000000000000000, 0.000000000000000000, 0.000000000000000000 ) ) ;
#5948 = CARTESIAN_POINT ( 'NONE',  ( -22.21770253897231839, -3.871672004621880436, -225.0000000000000000 ) ) ;
#5949 = DIRECTION ( 'NONE',  ( 0.000000000000000000, -1.000000000000000000, 0.000000000000000000 ) ) ;
#5950 = CARTESIAN_POINT ( 'NONE',  ( -8.000000000000003553, 100.3953136438507272, 10.00000000000000000 ) ) ;
#5951 = ORIENTED_EDGE ( 'NONE', *, *, #5032, .T. ) ;
#5952 = ORIENTED_EDGE ( 'NONE', *, *, #4211, .T. ) ;
#5953 = VECTOR ( 'NONE', #5335, 1000.000000000000000 ) ;
#5954 = CARTESIAN_POINT ( 'NONE',  ( 64.99991398172927859, 76.99999716619419132, 281.0000000000000000 ) ) ;
#5955 = FACE_OUTER_BOUND ( 'NONE', #3974, .T. ) ;
#5956 = CIRCLE ( 'NONE', #591, 22.67164836619068424 ) ;
#5957 = CARTESIAN_POINT ( 'NONE',  ( 0.000000000000000000, 0.000000000000000000, -20.00000000000000000 ) ) ;
#5958 = VERTEX_POINT ( 'NONE', #4138 ) ;
#5959 = AXIS2_PLACEMENT_3D ( 'NONE', #5991, #2560, #5564 ) ;
#5960 = DIRECTION ( 'NONE',  ( 1.000000000000000000, 0.000000000000000000, 0.000000000000000000 ) ) ;
#5961 = CARTESIAN_POINT ( 'NONE',  ( -2.012341796004660122, -19.89850447888114005, 39.00000000000001421 ) ) ;
#5962 = AXIS2_PLACEMENT_3D ( 'NONE', #4310, #2284, #1875 ) ;
#5963 = DIRECTION ( 'NONE',  ( -1.000000000000000000, 0.000000000000000000, 0.000000000000000000 ) ) ;
#5964 = ORIENTED_EDGE ( 'NONE', *, *, #1834, .F. ) ;
#5965 = CARTESIAN_POINT ( 'NONE',  ( 0.000000000000000000, 0.000000000000000000, -4.000000000000000000 ) ) ;
#5966 = CIRCLE ( 'NONE', #1854, 22.00000000000000000 ) ;
#5967 = DIRECTION ( 'NONE',  ( 0.000000000000000000, 0.000000000000000000, -1.000000000000000000 ) ) ;
#5968 = CIRCLE ( 'NONE', #416, 89.87058297576894006 ) ;
#5969 = DIRECTION ( 'NONE',  ( 1.000000000000000000, 0.000000000000000000, 0.000000000000000000 ) ) ;
#5970 = VECTOR ( 'NONE', #1086, 1000.000000000000000 ) ;
#5971 = LINE ( 'NONE', #3989, #1337 ) ;
#5972 = ORIENTED_EDGE ( 'NONE', *, *, #752, .F. ) ;
#5973 = LINE ( 'NONE', #5027, #3486 ) ;
#5974 = EDGE_LOOP ( 'NONE', ( #5482, #2868 ) ) ;
#5975 = CARTESIAN_POINT ( 'NONE',  ( 1.794389728719248733, 22.93422366650650090, 24.47880888172866065 ) ) ;
#5976 = AXIS2_PLACEMENT_3D ( 'NONE', #3340, #2854, #4830 ) ;
#5977 = DIRECTION ( 'NONE',  ( 1.000000000000000000, 0.000000000000000000, 0.000000000000000000 ) ) ;
#5978 = CARTESIAN_POINT ( 'NONE',  ( -174.7835321302054865, 68.75545066608756883, 9.999999999999996447 ) ) ;
#5979 = VECTOR ( 'NONE', #3306, 1000.000000000000000 ) ;
#5980 = ORIENTED_EDGE ( 'NONE', *, *, #5715, .T. ) ;
#5981 = ORIENTED_EDGE ( 'NONE', *, *, #4103, .F. ) ;
#5982 = EDGE_CURVE ( 'NONE', #2926, #4976, #1668, .T. ) ;
#5983 = CARTESIAN_POINT ( 'NONE',  ( 0.000000000000000000, 0.000000000000000000, -4.000000000000000000 ) ) ;
#5984 = CLOSED_SHELL ( 'NONE', ( #3823, #3720, #796, #6174, #2117, #3023, #4005, #1667, #3520, #4789, #4389, #3497, #5022, #3603, #3890, #3525, #5764, #255, #4068, #514, #5635, #1845, #466, #6299, #4563, #3342, #1116, #2730, #4838, #5732, #197 ) ) ;
#5985 = VECTOR ( 'NONE', #3303, 1000.000000000000000 ) ;
#5986 = EDGE_CURVE ( 'NONE', #1070, #371, #1639, .T. ) ;
#5987 = CARTESIAN_POINT ( 'NONE',  ( 12.54137761259614514, 29.87368101119752950, 2.025772336917471161 ) ) ;
#5988 = CARTESIAN_POINT ( 'NONE',  ( -16.00000000000000355, 0.000000000000000000, 16.00000000000000000 ) ) ;
#5989 = EDGE_CURVE ( 'NONE', #862, #2130, #1204, .T. ) ;
#5990 = EDGE_CURVE ( 'NONE', #4120, #3745, #3353, .T. ) ;
#5991 = CARTESIAN_POINT ( 'NONE',  ( 44.64065620456912598, 28.99954194078667413, -115.0000000000000000 ) ) ;
#5992 = ORIENTED_EDGE ( 'NONE', *, *, #1232, .F. ) ;
#5993 = AXIS2_PLACEMENT_3D ( 'NONE', #5948, #4767, #6251 ) ;
#5994 = CARTESIAN_POINT ( 'NONE',  ( -44.00000000000000000, -13.41640786499873350, -195.0000000000000000 ) ) ;
#5995 = CARTESIAN_POINT ( 'NONE',  ( -15.99408614349810698, -16.52843635781563592, 0.000000000000000000 ) ) ;
#5996 = ORIENTED_EDGE ( 'NONE', *, *, #5456, .T. ) ;
#5997 = DIRECTION ( 'NONE',  ( 1.000000000000000000, 0.000000000000000000, 0.000000000000000000 ) ) ;
#5998 = CARTESIAN_POINT ( 'NONE',  ( 0.000000000000000000, 0.000000000000000000, -4.000000000000000000 ) ) ;
#5999 = FACE_OUTER_BOUND ( 'NONE', #347, .T. ) ;
#6000 = VERTEX_POINT ( 'NONE', #3665 ) ;
#6001 = CARTESIAN_POINT ( 'NONE',  ( 12.82303992477784860, 19.09670753041942959, 4.547733370409773990 ) ) ;
#6002 = AXIS2_PLACEMENT_3D ( 'NONE', #5225, #2700, #2287 ) ;
#6003 = DIRECTION ( 'NONE',  ( -0.000000000000000000, -0.000000000000000000, -1.000000000000000000 ) ) ;
#6004 = CARTESIAN_POINT ( 'NONE',  ( 7.481756639719942648, 21.74910199390652465, 31.20551891105749931 ) ) ;
#6005 = CARTESIAN_POINT ( 'NONE',  ( -17.00000000000000000, 0.000000000000000000, -175.0000000000000284 ) ) ;
#6006 = ADVANCED_FACE ( 'NONE', ( #1216 ), #5576, .T. ) ;
#6007 = DIRECTION ( 'NONE',  ( 1.000000000000000000, 0.000000000000000000, 0.000000000000000000 ) ) ;
#6008 = ORIENTED_EDGE ( 'NONE', *, *, #2508, .T. ) ;
#6009 = ORIENTED_EDGE ( 'NONE', *, *, #4400, .F. ) ;
#6010 = VERTEX_POINT ( 'NONE', #3569 ) ;
#6011 = CARTESIAN_POINT ( 'NONE',  ( 265.0000000000000000, 14.00000000000000000, 110.0000000000000000 ) ) ;
#6012 = EDGE_CURVE ( 'NONE', #1881, #4328, #4800, .T. ) ;
#6013 = CARTESIAN_POINT ( 'NONE',  ( 13.41482486054668399, 26.39531364385071655, 5.999999999999990230 ) ) ;
#6014 = FACE_OUTER_BOUND ( 'NONE', #2029, .T. ) ;
#6015 = CARTESIAN_POINT ( 'NONE',  ( -7.500000000000000000, 0.000000000000000000, 1.000000000000000888 ) ) ;
#6016 = CARTESIAN_POINT ( 'NONE',  ( 0.000000000000000000, 0.000000000000000000, 0.000000000000000000 ) ) ;
#6017 = VERTEX_POINT ( 'NONE', #5122 ) ;
#6018 = EDGE_CURVE ( 'NONE', #1144, #3522, #2732, .T. ) ;
#6019 = EDGE_CURVE ( 'NONE', #5896, #3054, #3632, .T. ) ;
#6020 = CARTESIAN_POINT ( 'NONE',  ( 2.012341796004660122, 25.00000000000000000, 39.00000000000001421 ) ) ;
#6021 = CARTESIAN_POINT ( 'NONE',  ( 0.000000000000000000, 0.000000000000000000, -20.00000000000000000 ) ) ;
#6022 = VERTEX_POINT ( 'NONE', #4020 ) ;
#6023 = EDGE_CURVE ( 'NONE', #81, #434, #908, .T. ) ;
#6024 = CARTESIAN_POINT ( 'NONE',  ( -2.012341796004660122, 25.00000000000000000, 39.00000000000001421 ) ) ;
#6025 = VECTOR ( 'NONE', #6057, 1000.000000000000000 ) ;
#6026 = EDGE_CURVE ( 'NONE', #3408, #5800, #5023, .T. ) ;
#6027 = CARTESIAN_POINT ( 'NONE',  ( 6.500000000000000000, 0.000000000000000000, 47.00000000000000000 ) ) ;
#6028 = CIRCLE ( 'NONE', #3861, 21.00000000000000355 ) ;
#6029 = CARTESIAN_POINT ( 'NONE',  ( 0.3392246580399980727, -19.99999999999999645, 39.27501000028010480 ) ) ;
#6030 = EDGE_LOOP ( 'NONE', ( #4097, #2122, #1257, #3325, #1104, #63, #2003 ) ) ;
#6031 = EDGE_CURVE ( 'NONE', #1070, #2368, #4187, .T. ) ;
#6032 = CARTESIAN_POINT ( 'NONE',  ( -1.707452990153496275, 22.95315184250077323, 9.939577019203930774 ) ) ;
#6033 = DIRECTION ( 'NONE',  ( -1.000000000000000000, 0.000000000000000000, 0.000000000000000000 ) ) ;
#6034 = CARTESIAN_POINT ( 'NONE',  ( -7.443729366988918004E-21, 23.00000000000000000, 24.27501000028010125 ) ) ;
#6035 = PRESENTATION_LAYER_ASSIGNMENT (  '', '', ( #2430 ) ) ;
#6036 = CARTESIAN_POINT ( 'NONE',  ( 18.00000000000000355, 100.3953136438507272, 1.999999999999998224 ) ) ;
#6037 = CARTESIAN_POINT ( 'NONE',  ( -13.14183123006980480, 39.58265509608657595, -45.00000000000000000 ) ) ;
#6038 = VERTEX_POINT ( 'NONE', #3833 ) ;
#6039 = ORIENTED_EDGE ( 'NONE', *, *, #5341, .F. ) ;
#6040 = AXIS2_PLACEMENT_3D ( 'NONE', #5719, #5619, #4713 ) ;
#6041 = ORIENTED_EDGE ( 'NONE', *, *, #6179, .F. ) ;
#6042 = PLANE ( 'NONE',  #1567 ) ;
#6043 = VECTOR ( 'NONE', #4829, 1000.000000000000000 ) ;
#6044 = DIRECTION ( 'NONE',  ( -1.000000000000000000, 0.000000000000000000, 0.000000000000000000 ) ) ;
#6045 = CARTESIAN_POINT ( 'NONE',  ( 0.2052511266213280505, 21.25619793154159964, -240.0000000000000000 ) ) ;
#6046 = CARTESIAN_POINT ( 'NONE',  ( 0.000000000000000000, 0.000000000000000000, 41.00000000000000000 ) ) ;
#6047 = AXIS2_PLACEMENT_3D ( 'NONE', #2564, #3472, #5474 ) ;
#6048 = CARTESIAN_POINT ( 'NONE',  ( -13.14183123006980480, 39.58265509608657595, -30.00000000000000000 ) ) ;
#6049 = ORIENTED_EDGE ( 'NONE', *, *, #6179, .T. ) ;
#6050 = AXIS2_PLACEMENT_3D ( 'NONE', #4608, #5513, #237 ) ;
#6051 =( LENGTH_UNIT ( ) NAMED_UNIT ( * ) SI_UNIT ( .MILLI., .METRE. ) );
#6052 = DIRECTION ( 'NONE',  ( -0.000000000000000000, -0.000000000000000000, -1.000000000000000000 ) ) ;
#6053 = ORIENTED_EDGE ( 'NONE', *, *, #5505, .T. ) ;
#6054 = FACE_OUTER_BOUND ( 'NONE', #2715, .T. ) ;
#6055 = ORIENTED_EDGE ( 'NONE', *, *, #4483, .T. ) ;
#6056 = VECTOR ( 'NONE', #3923, 1000.000000000000000 ) ;
#6057 = DIRECTION ( 'NONE',  ( 0.000000000000000000, -1.000000000000000000, 0.000000000000000000 ) ) ;
#6058 = PRODUCT_DEFINITION_SHAPE ( 'NONE', 'NONE',  #1928 ) ;
#6059 = CARTESIAN_POINT ( 'NONE',  ( 0.000000000000000000, 0.000000000000000000, -175.0000000000000284 ) ) ;
#6060=STYLED_ITEM('',(#6398),#4588);
#6061 = FACE_OUTER_BOUND ( 'NONE', #3160, .T. ) ;
#6062 = DIRECTION ( 'NONE',  ( -1.000000000000000000, 0.000000000000000000, 0.000000000000000000 ) ) ;
#6063 = ORIENTED_EDGE ( 'NONE', *, *, #358, .T. ) ;
#6064 = ADVANCED_FACE ( 'NONE', ( #2694 ), #4795, .F. ) ;
#6065 = CARTESIAN_POINT ( 'NONE',  ( -0.8355139846970627282, 23.00151096327411793, 10.00195343045036189 ) ) ;
#6066 = VECTOR ( 'NONE', #1075, 1000.000000000000000 ) ;
#6067 = PRODUCT ( 'Part 32,5_Varsay\X2\0131\X0\lan', 'Part 32,5_Varsay\X2\0131\X0\lan', '', ( #159 ) ) ;
#6068 = CARTESIAN_POINT ( 'NONE',  ( 6.137861079775116302, 22.16774101882030124, 27.44213700196646144 ) ) ;
#6069 = VECTOR ( 'NONE', #4584, 1000.000000000000000 ) ;
#6070 = CARTESIAN_POINT ( 'NONE',  ( -0.4617977782627312178, 24.99947972102657445, 9.999268903951904264 ) ) ;
#6071 = CARTESIAN_POINT ( 'NONE',  ( 3.667391228670915382, -22.70656428659075843, 38.32101890234235242 ) ) ;
#6072 = EDGE_LOOP ( 'NONE', ( #4246, #3795, #3305, #3698 ) ) ;
#6073 = B_SPLINE_CURVE_WITH_KNOTS ( 'NONE', 3,
 ( #6034, #110, #2068, #4025, #2157, #5975, #2126, #594, #1577, #3518, #5547, #1554, #5485, #3638, #1091, #6068, #1067, #4082, #3033, #3155, #1610, #2546, #689, #1645, #6004, #3548, #5512, #3064, #2579, #1124, #4116, #5030, #3096, #5066, #656, #2638, #4606, #3188, #5747, #817, #5195, #4248, #3778, #3671 ),
 .UNSPECIFIED., .F., .F.,
 ( 4, 2, 2, 2, 2, 2, 2, 2, 2, 2, 2, 2, 2, 2, 2, 2, 2, 2, 2, 2, 2, 4 ),
 ( 0.02157941337148385624, 0.02225324431794266020, 0.02292707526440146415, 0.02427473715731907553, 0.02562239905023668690, 0.02697006094315429828, 0.02764389188961310223, 0.02831772283607190271, 0.02966538472898951062, 0.03033921567544831110, 0.03101304662190711506, 0.03236070851482472643, 0.03303453946128352692, 0.03370837040774233434, 0.03505603230065991449, 0.03640369419357750158, 0.03707752514003628125, 0.03775135608649506092, 0.03909901797941260637, 0.04044667987233015183, 0.04179434176524769728, 0.04314200365816523580 ),
 .UNSPECIFIED. ) ;
#6074 = VERTEX_POINT ( 'NONE', #2822 ) ;
#6075 = VECTOR ( 'NONE', #4022, 1000.000000000000000 ) ;
#6076 = DIRECTION ( 'NONE',  ( -1.000000000000000000, -1.852483853906148286E-16, 0.000000000000000000 ) ) ;
#6077 = FACE_BOUND ( 'NONE', #3684, .T. ) ;
#6078 = CARTESIAN_POINT ( 'NONE',  ( 13.14183123006966980, -39.58265509608656174, -115.0000000000000000 ) ) ;
#6079 = VECTOR ( 'NONE', #3276, 1000.000000000000000 ) ;
#6080 = DIRECTION ( 'NONE',  ( 0.000000000000000000, 0.000000000000000000, 1.000000000000000000 ) ) ;
#6081 = CARTESIAN_POINT ( 'NONE',  ( 12.50000000000001421, 120.0000000000000000, -4.000000000000000000 ) ) ;
#6082 = ORIENTED_EDGE ( 'NONE', *, *, #1247, .F. ) ;
#6083 = CYLINDRICAL_SURFACE ( 'NONE', #1813, 7.500000000000000000 ) ;
#6084 = ORIENTED_EDGE ( 'NONE', *, *, #1048, .T. ) ;
#6085 = CARTESIAN_POINT ( 'NONE',  ( -25.00000000000000000, 0.000000000000000000, 55.00000000000000711 ) ) ;
#6086 = CIRCLE ( 'NONE', #4958, 23.00000000000000000 ) ;
#6087 = SURFACE_SIDE_STYLE ('',( #6220 ) ) ;
#6088 = CARTESIAN_POINT ( 'NONE',  ( 0.000000000000000000, 14.00000000000000000, 110.0000000000000000 ) ) ;
#6089 = ADVANCED_FACE ( 'NONE', ( #5804 ), #4171, .T. ) ;
#6090 = CARTESIAN_POINT ( 'NONE',  ( 22.00000000000000000, 2.694222958124176809E-15, 50.00000000000000711 ) ) ;
#6091 = PLANE ( 'NONE',  #731 ) ;
#6092 = ORIENTED_EDGE ( 'NONE', *, *, #2739, .F. ) ;
#6093 = SURFACE_SIDE_STYLE ('',( #1256 ) ) ;
#6094 = EDGE_CURVE ( 'NONE', #6280, #4938, #6149, .T. ) ;
#6095 = CYLINDRICAL_SURFACE ( 'NONE', #5884, 16.00000000000000000 ) ;
#6096 = CARTESIAN_POINT ( 'NONE',  ( -7.443729366988918004E-21, 23.00000000000000000, 24.27501000028010125 ) ) ;
#6097 = CARTESIAN_POINT ( 'NONE',  ( -4.322439664174057228, 24.63752030717468600, 9.487820034421872606 ) ) ;
#6098 = CARTESIAN_POINT ( 'NONE',  ( 5.723282545231354490, -22.27700230555918992, 36.62722877095559681 ) ) ;
#6099 = VERTEX_POINT ( 'NONE', #292 ) ;
#6100 = ORIENTED_EDGE ( 'NONE', *, *, #104, .F. ) ;
#6101 = ORIENTED_EDGE ( 'NONE', *, *, #3331, .T. ) ;
#6102 = CARTESIAN_POINT ( 'NONE',  ( -43.99999999999987921, 13.41640786499904969, -115.0000000000000000 ) ) ;
#6103 = AXIS2_PLACEMENT_3D ( 'NONE', #5128, #6229, #6125 ) ;
#6104 = DIRECTION ( 'NONE',  ( -0.000000000000000000, -0.000000000000000000, 1.000000000000000000 ) ) ;
#6105 = EDGE_CURVE ( 'NONE', #3220, #1488, #6345, .T. ) ;
#6106 = DIRECTION ( 'NONE',  ( 0.000000000000000000, -1.000000000000000000, 0.000000000000000000 ) ) ;
#6107 = FACE_OUTER_BOUND ( 'NONE', #2163, .T. ) ;
#6108 = DIRECTION ( 'NONE',  ( -0.000000000000000000, 0.000000000000000000, -1.000000000000000000 ) ) ;
#6109 = ORIENTED_EDGE ( 'NONE', *, *, #2547, .F. ) ;
#6110 = CARTESIAN_POINT ( 'NONE',  ( 0.000000000000000000, 0.000000000000000000, -175.0000000000000000 ) ) ;
#6111 = CARTESIAN_POINT ( 'NONE',  ( -14.35983982790937219, -17.97565917864960738, 2.741545323018244940 ) ) ;
#6112 = ORIENTED_EDGE ( 'NONE', *, *, #3690, .F. ) ;
#6113 = PRODUCT_DEFINITION_SHAPE ( 'NONE', 'NONE',  #1725 ) ;
#6114 = DIRECTION ( 'NONE',  ( -0.000000000000000000, -0.000000000000000000, 1.000000000000000000 ) ) ;
#6115 = VERTEX_POINT ( 'NONE', #3339 ) ;
#6116 = PRODUCT_DEFINITION_FORMATION_WITH_SPECIFIED_SOURCE ( 'ANY', '', #1681, .NOT_KNOWN. ) ;
#6117 = UNCERTAINTY_MEASURE_WITH_UNIT (LENGTH_MEASURE( 1.000000000000000082E-05 ), #4863, 'distance_accuracy_value', 'NONE');
#6118 =( NAMED_UNIT ( * ) SI_UNIT ( $, .STERADIAN. ) SOLID_ANGLE_UNIT ( ) );
#6119 = DIRECTION ( 'NONE',  ( -1.000000000000000000, 0.000000000000000000, -0.000000000000000000 ) ) ;
#6120 = DIRECTION ( 'NONE',  ( 1.000000000000000000, 0.000000000000000000, 0.000000000000000000 ) ) ;
#6121 = DIRECTION ( 'NONE',  ( -1.000000000000000000, 0.000000000000000000, 0.000000000000000000 ) ) ;
#6122 = ORIENTED_EDGE ( 'NONE', *, *, #3334, .F. ) ;
#6123 = CARTESIAN_POINT ( 'NONE',  ( 0.9177768309508191891, 22.98591141273915639, 9.981795115530772478 ) ) ;
#6124 = PRESENTATION_STYLE_ASSIGNMENT (( #3063 ) ) ;
#6125 = DIRECTION ( 'NONE',  ( -1.000000000000000000, 0.000000000000000000, 0.000000000000000000 ) ) ;
#6126 = CARTESIAN_POINT ( 'NONE',  ( -15.99408614349810698, 19.21429697996681796, -4.336808689942017736E-15 ) ) ;
#6127 = CARTESIAN_POINT ( 'NONE',  ( 2.869322346082823660, -22.82391999846087316, 38.71877048136666843 ) ) ;
#6128 = ORIENTED_EDGE ( 'NONE', *, *, #4546, .F. ) ;
#6129 = CIRCLE ( 'NONE', #166, 6.500000000000005329 ) ;
#6130 = VERTEX_POINT ( 'NONE', #1736 ) ;
#6131 = DIRECTION ( 'NONE',  ( -0.000000000000000000, -0.000000000000000000, -1.000000000000000000 ) ) ;
#6132 = CARTESIAN_POINT ( 'NONE',  ( 6.500000000000000000, 0.000000000000000000, 0.000000000000000000 ) ) ;
#6133 = CARTESIAN_POINT ( 'NONE',  ( 15.99408614349810698, 25.00000000000000000, 0.000000000000000000 ) ) ;
#6134 = PLANE ( 'NONE',  #3589 ) ;
#6135 = VECTOR ( 'NONE', #4979, 1000.000000000000000 ) ;
#6136 = AXIS2_PLACEMENT_3D ( 'NONE', #5350, #4824, #6314 ) ;
#6137 = ORIENTED_EDGE ( 'NONE', *, *, #1591, .T. ) ;
#6138 = CARTESIAN_POINT ( 'NONE',  ( 18.00000000000001421, 30.39531364385072010, 1.999999999999989564 ) ) ;
#6139 = ORIENTED_EDGE ( 'NONE', *, *, #2739, .T. ) ;
#6140 = CARTESIAN_POINT ( 'NONE',  ( 15.63674378938990905, -16.87422613917171432, 0.7336288283346513728 ) ) ;
#6141 = ORIENTED_EDGE ( 'NONE', *, *, #3413, .F. ) ;
#6142 = CARTESIAN_POINT ( 'NONE',  ( 0.2052511266213280505, 21.25619793154159964, 0.000000000000000000 ) ) ;
#6143 = EDGE_LOOP ( 'NONE', ( #3302, #4777, #3595, #4493 ) ) ;
#6144 = AXIS2_PLACEMENT_3D ( 'NONE', #2425, #17, #3456 ) ;
#6145 = DIRECTION ( 'NONE',  ( -1.000000000000000000, 0.000000000000000000, 0.000000000000000000 ) ) ;
#6146 = DIRECTION ( 'NONE',  ( 0.000000000000000000, 1.000000000000000000, 0.000000000000000000 ) ) ;
#6147 = DIRECTION ( 'NONE',  ( -0.000000000000000000, 0.000000000000000000, -1.000000000000000000 ) ) ;
#6148 = ADVANCED_FACE ( 'NONE', ( #2281 ), #3247, .T. ) ;
#6149 = LINE ( 'NONE', #1378, #5019 ) ;
#6150 = AXIS2_PLACEMENT_3D ( 'NONE', #6027, #1604, #5219 ) ;
#6151 = CARTESIAN_POINT ( 'NONE',  ( 0.000000000000000000, 0.000000000000000000, -248.0000000000000000 ) ) ;
#6152 = ORIENTED_EDGE ( 'NONE', *, *, #5990, .T. ) ;
#6153 = CARTESIAN_POINT ( 'NONE',  ( -5.943311860187945328, 22.23481035324009270, 8.999810584836245297 ) ) ;
#6154 = ORIENTED_EDGE ( 'NONE', *, *, #5059, .T. ) ;
#6155 = CARTESIAN_POINT ( 'NONE',  ( 6.734764818747090764, 24.07658780463484405, 35.11236497522016720 ) ) ;
#6156 = FACE_OUTER_BOUND ( 'NONE', #3319, .T. ) ;
#6157 = CIRCLE ( 'NONE', #1532, 17.00000000000000000 ) ;
#6158 = CARTESIAN_POINT ( 'NONE',  ( 12.76907600075765536, 21.49559483975649243, 4.603672158788648439 ) ) ;
#6159 = CARTESIAN_POINT ( 'NONE',  ( 7.512701611559312376, -21.73844013154226218, 31.66439142681324981 ) ) ;
#6160 = VERTEX_POINT ( 'NONE', #2797 ) ;
#6161 = PRESENTATION_LAYER_ASSIGNMENT (  '', '', ( #5447 ) ) ;
#6162 = EDGE_CURVE ( 'NONE', #6160, #4541, #3703, .T. ) ;
#6163 = ORIENTED_EDGE ( 'NONE', *, *, #1205, .T. ) ;
#6164 = FACE_OUTER_BOUND ( 'NONE', #4301, .T. ) ;
#6165 = CIRCLE ( 'NONE', #3382, 12.50000000000001421 ) ;
#6166 = AXIS2_PLACEMENT_3D ( 'NONE', #3648, #667, #182 ) ;
#6167 = PRODUCT_DEFINITION_SHAPE ( 'NONE', 'NONE',  #2008 ) ;
#6168 = CARTESIAN_POINT ( 'NONE',  ( 174.7835321302054865, 68.75545066608756883, 0.000000000000000000 ) ) ;
#6169 = DIRECTION ( 'NONE',  ( -0.000000000000000000, -0.000000000000000000, 1.000000000000000000 ) ) ;
#6170 = CARTESIAN_POINT ( 'NONE',  ( 59.99991398172927859, 76.99999716619419132, 5.000000000000000000 ) ) ;
#6171 = ADVANCED_FACE ( 'NONE', ( #4242 ), #2722, .T. ) ;
#6172 = AXIS2_PLACEMENT_3D ( 'NONE', #4380, #11, #3446 ) ;
#6173 = ORIENTED_EDGE ( 'NONE', *, *, #5527, .F. ) ;
#6174 = ADVANCED_FACE ( 'NONE', ( #3215 ), #3310, .T. ) ;
#6175 = CARTESIAN_POINT ( 'NONE',  ( 16.23652742703164975, 37.28747423195200383, -180.0000000000000000 ) ) ;
#6176 = ORIENTED_EDGE ( 'NONE', *, *, #4768, .F. ) ;
#6177 = EDGE_CURVE ( 'NONE', #3054, #2143, #2345, .T. ) ;
#6178 = FACE_OUTER_BOUND ( 'NONE', #3752, .T. ) ;
#6179 = EDGE_CURVE ( 'NONE', #990, #1518, #896, .T. ) ;
#6180 = ADVANCED_FACE ( 'NONE', ( #4769, #1872 ), #6222, .F. ) ;
#6181 = CARTESIAN_POINT ( 'NONE',  ( 4.293665609699220731, -22.59978795717626454, 9.479591363866271436 ) ) ;
#6182 = ORIENTED_EDGE ( 'NONE', *, *, #28, .F. ) ;
#6183 = CARTESIAN_POINT ( 'NONE',  ( 9.184850993605147944E-16, 25.00000000000000000, 39.27501000028010480 ) ) ;
#6184 = ORIENTED_EDGE ( 'NONE', *, *, #3045, .T. ) ;
#6185 = DIRECTION ( 'NONE',  ( -1.000000000000000000, 0.000000000000000000, 0.000000000000000000 ) ) ;
#6186 = AXIS2_PLACEMENT_3D ( 'NONE', #3041, #2557, #4489 ) ;
#6187 = DIRECTION ( 'NONE',  ( 1.000000000000000000, 0.000000000000000000, 0.000000000000000000 ) ) ;
#6188 = DIRECTION ( 'NONE',  ( -0.000000000000000000, 0.000000000000000000, 1.000000000000000000 ) ) ;
#6189 = EDGE_CURVE ( 'NONE', #3396, #4872, #1803, .T. ) ;
#6190 = CARTESIAN_POINT ( 'NONE',  ( -6.737723522270822940, -24.07574026236370202, 28.44448745219711583 ) ) ;
#6191 = ORIENTED_EDGE ( 'NONE', *, *, #791, .F. ) ;
#6192 = DIRECTION ( 'NONE',  ( 1.000000000000000000, 0.000000000000000000, 0.000000000000000000 ) ) ;
#6193 = ORIENTED_EDGE ( 'NONE', *, *, #752, .T. ) ;
#6194 = CARTESIAN_POINT ( 'NONE',  ( 42.00000000000000000, 69.00000000000000000, 0.000000000000000000 ) ) ;
#6195 = CARTESIAN_POINT ( 'NONE',  ( 0.000000000000000000, 69.00000000000000000, 110.0000000000000000 ) ) ;
#6196 = AXIS2_PLACEMENT_3D ( 'NONE', #681, #2119, #1524 ) ;
#6197 = CARTESIAN_POINT ( 'NONE',  ( -13.14183123006980480, 39.58265509608657595, -195.0000000000000000 ) ) ;
#6198 = CARTESIAN_POINT ( 'NONE',  ( 1.710351842506662612, -24.94259032362968398, 24.46851125284992889 ) ) ;
#6199 = ORIENTED_EDGE ( 'NONE', *, *, #6309, .T. ) ;
#6200 = VERTEX_POINT ( 'NONE', #1352 ) ;
#6201 = CYLINDRICAL_SURFACE ( 'NONE', #2087, 89.87058297576894006 ) ;
#6202 = ADVANCED_FACE ( 'NONE', ( #3771 ), #1282, .F. ) ;
#6203 = CARTESIAN_POINT ( 'NONE',  ( 237.0000000000000284, 68.99999999999997158, 110.0000000000000000 ) ) ;
#6204 = DIRECTION ( 'NONE',  ( -0.000000000000000000, -0.000000000000000000, 1.000000000000000000 ) ) ;
#6205 = DIRECTION ( 'NONE',  ( 1.000000000000000000, 0.000000000000000000, 0.000000000000000000 ) ) ;
#6206 = ORIENTED_EDGE ( 'NONE', *, *, #8, .T. ) ;
#6207 = ORIENTED_EDGE ( 'NONE', *, *, #2097, .T. ) ;
#6208 = CIRCLE ( 'NONE', #2502, 17.00000000000000000 ) ;
#6209 = EDGE_CURVE ( 'NONE', #1569, #2747, #1607, .T. ) ;
#6210 = EDGE_CURVE ( 'NONE', #4556, #6130, #4522, .T. ) ;
#6211 = CONTEXT_DEPENDENT_SHAPE_REPRESENTATION ( #1514, #3696 ) ;
#6212 = CARTESIAN_POINT ( 'NONE',  ( -13.09536939405042055, -18.91069771112636744, 4.258167217702273355 ) ) ;
#6213 = CARTESIAN_POINT ( 'NONE',  ( -25.00000000000000000, 0.000000000000000000, 41.00000000000000000 ) ) ;
#6214 = ORIENTED_EDGE ( 'NONE', *, *, #222, .F. ) ;
#6215 = DIRECTION ( 'NONE',  ( -0.000000000000000000, -0.000000000000000000, 1.000000000000000000 ) ) ;
#6216 = EDGE_LOOP ( 'NONE', ( #5260, #4121, #432, #4358 ) ) ;
#6217 = EDGE_CURVE ( 'NONE', #5105, #4956, #4908, .T. ) ;
#6218 =( REPRESENTATION_RELATIONSHIP ('NONE','NONE', #632, #1490 ) REPRESENTATION_RELATIONSHIP_WITH_TRANSFORMATION ( #893 )SHAPE_REPRESENTATION_RELATIONSHIP( ) );
#6219 = EDGE_CURVE ( 'NONE', #4140, #5682, #3558, .T. ) ;
#6220 = SURFACE_STYLE_FILL_AREA ( #2753 ) ;
#6221 = CARTESIAN_POINT ( 'NONE',  ( -1.331801922117356663E-14, -72.49991987048069575, 281.0000000000000000 ) ) ;
#6222 = PLANE ( 'NONE',  #4488 ) ;
#6223 = EDGE_CURVE ( 'NONE', #5286, #2807, #1512, .T. ) ;
#6224 = CARTESIAN_POINT ( 'NONE',  ( -7.487557334333946102, -23.85240338065037236, 32.27275042597646859 ) ) ;
#6225 = ORIENTED_EDGE ( 'NONE', *, *, #2721, .F. ) ;
#6226 = LINE ( 'NONE', #1808, #919 ) ;
#6227 = VERTEX_POINT ( 'NONE', #6015 ) ;
#6228 = CARTESIAN_POINT ( 'NONE',  ( 6.737723522270820276, 24.07574026236370912, 28.44448745219711583 ) ) ;
#6229 = DIRECTION ( 'NONE',  ( 0.000000000000000000, 0.000000000000000000, -1.000000000000000000 ) ) ;
#6230 = ADVANCED_FACE ( 'NONE', ( #1102 ), #1965, .T. ) ;
#6231 = FACE_BOUND ( 'NONE', #1063, .T. ) ;
#6232 = CARTESIAN_POINT ( 'NONE',  ( 6.703346455576358665, -22.00175929117281015, 28.40382332099657958 ) ) ;
#6233 = ORIENTED_EDGE ( 'NONE', *, *, #5072, .F. ) ;
#6234 = ORIENTED_EDGE ( 'NONE', *, *, #2000, .F. ) ;
#6235 = DIRECTION ( 'NONE',  ( -0.000000000000000000, 0.000000000000000000, -1.000000000000000000 ) ) ;
#6236 = DIRECTION ( 'NONE',  ( -0.000000000000000000, -0.000000000000000000, 1.000000000000000000 ) ) ;
#6237 = AXIS2_PLACEMENT_3D ( 'NONE', #2059, #650, #1513 ) ;
#6238 = FACE_OUTER_BOUND ( 'NONE', #1095, .T. ) ;
#6239 = VECTOR ( 'NONE', #2655, 1000.000000000000000 ) ;
#6240 = ORIENTED_EDGE ( 'NONE', *, *, #2483, .T. ) ;
#6241 = EDGE_LOOP ( 'NONE', ( #1663, #1255, #212, #3565 ) ) ;
#6242 = DIRECTION ( 'NONE',  ( 1.000000000000000000, 0.000000000000000000, 0.000000000000000000 ) ) ;
#6243 = VECTOR ( 'NONE', #1682, 1000.000000000000000 ) ;
#6244 = AXIS2_PLACEMENT_3D ( 'NONE', #3244, #841, #5216 ) ;
#6245 = CARTESIAN_POINT ( 'NONE',  ( -13.30659111572999720, 26.80965796039522431, 7.792318603440349989 ) ) ;
#6246 = DIRECTION ( 'NONE',  ( 0.000000000000000000, -0.000000000000000000, 1.000000000000000000 ) ) ;
#6247 = EDGE_LOOP ( 'NONE', ( #4251, #854, #5681, #3980 ) ) ;
#6248 = CARTESIAN_POINT ( 'NONE',  ( 17.00000000000000000, 0.000000000000000000, -49.99999999999999289 ) ) ;
#6249 = EDGE_CURVE ( 'NONE', #3522, #4666, #4034, .T. ) ;
#6250 = AXIS2_PLACEMENT_3D ( 'NONE', #2888, #3435, #2955 ) ;
#6251 = DIRECTION ( 'NONE',  ( 1.000000000000000000, 0.000000000000000000, 0.000000000000000000 ) ) ;
#6252 = CARTESIAN_POINT ( 'NONE',  ( -17.00000000000000000, 0.000000000000000000, 48.00000000000000000 ) ) ;
#6253 = FACE_OUTER_BOUND ( 'NONE', #2208, .T. ) ;
#6254 = EDGE_LOOP ( 'NONE', ( #5811, #5200, #1598, #1328 ) ) ;
#6255 = DIRECTION ( 'NONE',  ( 0.000000000000000000, 0.000000000000000000, -1.000000000000000000 ) ) ;
#6256 = AXIS2_PLACEMENT_3D ( 'NONE', #3846, #3817, #6267 ) ;
#6257 = CARTESIAN_POINT ( 'NONE',  ( 4.580917930799680349, 24.58016474715297051, 37.73350732204200852 ) ) ;
#6258 = LINE ( 'NONE', #4280, #1778 ) ;
#6259 = AXIS2_PLACEMENT_3D ( 'NONE', #1291, #2254, #819 ) ;
#6260 = FACE_OUTER_BOUND ( 'NONE', #354, .T. ) ;
#6261 = CARTESIAN_POINT ( 'NONE',  ( -2.546401178541497462E-16, -25.00000000000000000, 24.27501000028010125 ) ) ;
#6262 = ORIENTED_EDGE ( 'NONE', *, *, #5104, .T. ) ;
#6263 = VECTOR ( 'NONE', #4196, 1000.000000000000000 ) ;
#6264 = VERTEX_POINT ( 'NONE', #2890 ) ;
#6265 = CARTESIAN_POINT ( 'NONE',  ( -6.493108461366345452, 24.14236833790515036, 35.53659098058280108 ) ) ;
#6266 = CARTESIAN_POINT ( 'NONE',  ( 18.00000000000001421, 30.39531364385072010, 9.999999999999991118 ) ) ;
#6267 = DIRECTION ( 'NONE',  ( 1.000000000000000000, 0.000000000000000000, -0.000000000000000000 ) ) ;
#6268 = CIRCLE ( 'NONE', #3689, 12.50000000000001421 ) ;
#6269 = CARTESIAN_POINT ( 'NONE',  ( -44.43364355155666345, 29.42304313293565343, -175.0000000000000284 ) ) ;
#6270 = ORIENTED_EDGE ( 'NONE', *, *, #2310, .F. ) ;
#6271 = ORIENTED_EDGE ( 'NONE', *, *, #4353, .T. ) ;
#6272 = ORIENTED_EDGE ( 'NONE', *, *, #5839, .T. ) ;
#6273 = AXIS2_PLACEMENT_3D ( 'NONE', #1139, #5177, #765 ) ;
#6274 = AXIS2_PLACEMENT_3D ( 'NONE', #124, #572, #5925 ) ;
#6275 = CARTESIAN_POINT ( 'NONE',  ( 25.00000000000000000, 3.061616997868383043E-15, 47.00000000000000711 ) ) ;
#6276 = CONTEXT_DEPENDENT_SHAPE_REPRESENTATION ( #1389, #723 ) ;
#6277 = LINE ( 'NONE', #3792, #1108 ) ;
#6278 = CIRCLE ( 'NONE', #3496, 22.67164836619066648 ) ;
#6279 = DIRECTION ( 'NONE',  ( 1.000000000000000000, 0.000000000000000000, 0.000000000000000000 ) ) ;
#6280 = VERTEX_POINT ( 'NONE', #1899 ) ;
#6281 = AXIS2_PLACEMENT_3D ( 'NONE', #257, #1642, #6121 ) ;
#6282 = DIRECTION ( 'NONE',  ( -1.000000000000000000, 0.000000000000000000, 0.000000000000000000 ) ) ;
#6283 = CARTESIAN_POINT ( 'NONE',  ( 2.449293599978538004E-15, 0.000000000000000000, 63.77501000028010480 ) ) ;
#6284 = CARTESIAN_POINT ( 'NONE',  ( 0.000000000000000000, 0.000000000000000000, 12.00000000000000000 ) ) ;
#6285 = AXIS2_PLACEMENT_3D ( 'NONE', #3983, #4894, #4861 ) ;
#6286 = CARTESIAN_POINT ( 'NONE',  ( -0.4912064067414951829, -25.00000000000000355, 39.27501000028010480 ) ) ;
#6287 = EDGE_LOOP ( 'NONE', ( #755, #3950, #1286, #2979 ) ) ;
#6288 = CARTESIAN_POINT ( 'NONE',  ( 279.0000000000000000, 68.99999999999997158, 110.0000000000000000 ) ) ;
#6289 = AXIS2_PLACEMENT_3D ( 'NONE', #1862, #2816, #1343 ) ;
#6290 = CARTESIAN_POINT ( 'NONE',  ( -22.21770253897380343, -3.871672004622680241, -195.0000000000000000 ) ) ;
#6291 = EDGE_CURVE ( 'NONE', #1805, #3965, #4491, .T. ) ;
#6292 = EDGE_CURVE ( 'NONE', #673, #3260, #2335, .T. ) ;
#6293 = DIRECTION ( 'NONE',  ( -0.000000000000000000, -0.000000000000000000, -1.000000000000000000 ) ) ;
#6294 = CARTESIAN_POINT ( 'NONE',  ( 5.133479616427196746, -24.46790356832290669, 26.30175839968469731 ) ) ;
#6295 = ORIENTED_EDGE ( 'NONE', *, *, #29, .T. ) ;
#6296 = CARTESIAN_POINT ( 'NONE',  ( -16.23652742703189489, -37.28747423195188304, -115.0000000000000000 ) ) ;
#6297 = ORIENTED_EDGE ( 'NONE', *, *, #5146, .T. ) ;
#6298 = DIRECTION ( 'NONE',  ( -0.000000000000000000, -0.000000000000000000, -1.000000000000000000 ) ) ;
#6299 = ADVANCED_FACE ( 'NONE', ( #2, #5411 ), #2106, .F. ) ;
#6300 = AXIS2_PLACEMENT_3D ( 'NONE', #4170, #1871, #777 ) ;
#6301 = DIRECTION ( 'NONE',  ( -3.903561672282183340E-16, 1.000000000000000000, -0.000000000000000000 ) ) ;
#6302 = CARTESIAN_POINT ( 'NONE',  ( 0.000000000000000000, 76.99999716619419132, 5.000000000000000000 ) ) ;
#6303 = CARTESIAN_POINT ( 'NONE',  ( 0.000000000000000000, 0.000000000000000000, 0.000000000000000000 ) ) ;
#6304 = EDGE_CURVE ( 'NONE', #1433, #3054, #1710, .T. ) ;
#6305 = EDGE_LOOP ( 'NONE', ( #3427, #5634 ) ) ;
#6306 = ORIENTED_EDGE ( 'NONE', *, *, #3991, .T. ) ;
#6307 = EDGE_CURVE ( 'NONE', #5846, #4913, #5872, .T. ) ;
#6308 = DIRECTION ( 'NONE',  ( 0.000000000000000000, 0.000000000000000000, 1.000000000000000000 ) ) ;
#6309 = EDGE_CURVE ( 'NONE', #5632, #2926, #5429, .T. ) ;
#6310 = CARTESIAN_POINT ( 'NONE',  ( -43.99999999999987921, 13.41640786499904969, -130.0000000000000000 ) ) ;
#6311 = ADVANCED_FACE ( 'NONE', ( #1000 ), #4925, .T. ) ;
#6312 = FACE_BOUND ( 'NONE', #2183, .T. ) ;
#6313 = ORIENTED_EDGE ( 'NONE', *, *, #1732, .F. ) ;
#6314 = DIRECTION ( 'NONE',  ( 1.000000000000000000, 0.000000000000000000, 0.000000000000000000 ) ) ;
#6315 =( NAMED_UNIT ( * ) SI_UNIT ( $, .STERADIAN. ) SOLID_ANGLE_UNIT ( ) );
#6316 = CARTESIAN_POINT ( 'NONE',  ( -6.703552034654557623, -22.00169986843530268, 28.40415011795442979 ) ) ;
#6317 = DIRECTION ( 'NONE',  ( 0.000000000000000000, 0.000000000000000000, 1.000000000000000000 ) ) ;
#6318 = CARTESIAN_POINT ( 'NONE',  ( 17.00000000000000000, 0.000000000000000000, -115.0000000000000000 ) ) ;
#6319 = VERTEX_POINT ( 'NONE', #1448 ) ;
#6320 = DIRECTION ( 'NONE',  ( -3.903561672282183340E-16, 1.000000000000000000, 0.000000000000000000 ) ) ;
#6321 = DIRECTION ( 'NONE',  ( 0.000000000000000000, 0.000000000000000000, 1.000000000000000000 ) ) ;
#6322 = DIRECTION ( 'NONE',  ( -0.000000000000000000, -0.000000000000000000, 1.000000000000000000 ) ) ;
#6323 = CARTESIAN_POINT ( 'NONE',  ( 7.101515257722367025, -23.97027555112599728, 29.35032263750039760 ) ) ;
#6324 = VERTEX_POINT ( 'NONE', #5386 ) ;
#6325 = DIRECTION ( 'NONE',  ( -0.000000000000000000, -0.000000000000000000, -1.000000000000000000 ) ) ;
#6326 = ORIENTED_EDGE ( 'NONE', *, *, #3245, .F. ) ;
#6327 = CYLINDRICAL_SURFACE ( 'NONE', #4131, 17.00000000000000000 ) ;
#6328 = CARTESIAN_POINT ( 'NONE',  ( -17.00000000000000355, -24.99999999999999645, -95.00000000000000000 ) ) ;
#6329 = DIRECTION ( 'NONE',  ( 1.000000000000000000, 0.000000000000000000, 0.000000000000000000 ) ) ;
#6330 = DIRECTION ( 'NONE',  ( 1.000000000000000000, 0.000000000000000000, -0.000000000000000000 ) ) ;
#6331 = EDGE_LOOP ( 'NONE', ( #1529, #1874, #3848, #5145 ) ) ;
#6332 = ORIENTED_EDGE ( 'NONE', *, *, #4270, .F. ) ;
#6333 = DIRECTION ( 'NONE',  ( -1.000000000000000000, -1.852483853906148040E-16, 0.000000000000000000 ) ) ;
#6334 = CARTESIAN_POINT ( 'NONE',  ( 0.000000000000000000, 0.000000000000000000, 41.00000000000000000 ) ) ;
#6335 = CIRCLE ( 'NONE', #4054, 16.00000000000000355 ) ;
#6336 = CARTESIAN_POINT ( 'NONE',  ( -5.896395598744651245, -24.30897383879704066, 9.016004279442030978 ) ) ;
#6337 = ORIENTED_EDGE ( 'NONE', *, *, #1323, .F. ) ;
#6338 = LINE ( 'NONE', #1445, #1188 ) ;
#6339 = CARTESIAN_POINT ( 'NONE',  ( -6.383431969492757929, -22.09754339782970334, 27.81230622618427617 ) ) ;
#6340 = DIRECTION ( 'NONE',  ( -0.000000000000000000, -0.000000000000000000, -1.000000000000000000 ) ) ;
#6341 = DIRECTION ( 'NONE',  ( -1.000000000000000000, 0.000000000000000000, -0.000000000000000000 ) ) ;
#6342 = ORIENTED_EDGE ( 'NONE', *, *, #5069, .T. ) ;
#6343 = CIRCLE ( 'NONE', #2834, 23.00000000000000000 ) ;
#6344 = FACE_OUTER_BOUND ( 'NONE', #2703, .T. ) ;
#6345 = CIRCLE ( 'NONE', #4293, 46.00000000000000000 ) ;
#6346 = DIRECTION ( 'NONE',  ( -0.000000000000000000, -0.000000000000000000, 1.000000000000000000 ) ) ;
#6347 = FACE_OUTER_BOUND ( 'NONE', #6305, .T. ) ;
#6348 = DIRECTION ( 'NONE',  ( -0.000000000000000000, -0.000000000000000000, 1.000000000000000000 ) ) ;
#6349 = AXIS2_PLACEMENT_3D ( 'NONE', #290, #2242, #4169 ) ;
#6350 = CARTESIAN_POINT ( 'NONE',  ( 0.000000000000000000, 0.000000000000000000, 48.00000000000000000 ) ) ;
#6351 = ORIENTED_EDGE ( 'NONE', *, *, #2867, .F. ) ;
#6352 = DIRECTION ( 'NONE',  ( -0.000000000000000000, 0.000000000000000000, -1.000000000000000000 ) ) ;
#6353 = DIRECTION ( 'NONE',  ( -0.000000000000000000, -0.000000000000000000, -1.000000000000000000 ) ) ;
#6354 = DIRECTION ( 'NONE',  ( -0.000000000000000000, -0.000000000000000000, -1.000000000000000000 ) ) ;
#6355 = B_SPLINE_CURVE_WITH_KNOTS ( 'NONE', 3,
 ( #6261, #883, #4708, #6198, #2387, #1847, #2830, #820, #1292, #3317, #4347, #1325, #6294, #3750, #4250, #5269, #4775, #1385, #6323, #5365, #304, #4744, #2357, #4805, #369, #3866, #2768, #403, #1880, #2324, #1905, #2290, #5297, #4283, #4317, #4225, #3259, #3780, #3291, #3347, #3809, #2033, #1549, #1459, #2448, #1007 ),
 .UNSPECIFIED., .F., .F.,
 ( 4, 2, 2, 2, 2, 2, 2, 2, 2, 2, 2, 2, 2, 2, 2, 2, 2, 2, 2, 2, 2, 2, 4 ),
 ( 2.472553540688041407E-19, 0.001474063385043937338, 0.002211095077565906116, 0.002948126770087874677, 0.004422190155131812232, 0.005159221847653780793, 0.005896253540175749354, 0.007370316925219684741, 0.008844380310263619260, 0.009581412002785590423, 0.01031844369530756506, 0.01179250708035150912, 0.01326657046539545318, 0.01474063385043939897, 0.01547766554296138054, 0.01621469723548336211, 0.01695172892800534195, 0.01768876062052732526, 0.01916282400557130575, 0.02063688739061528971, 0.02211095077565927366, 0.02284798246818127085, 0.02358501416070326456 ),
 .UNSPECIFIED. ) ;
#6356 = CARTESIAN_POINT ( 'NONE',  ( 279.0000000000000000, 68.99999999999997158, 110.0000000000000000 ) ) ;
#6357 = CARTESIAN_POINT ( 'NONE',  ( 0.000000000000000000, 0.000000000000000000, 16.00000000000000000 ) ) ;
#6358 = EDGE_CURVE ( 'NONE', #5091, #5198, #969, .T. ) ;
#6359 = CARTESIAN_POINT ( 'NONE',  ( -44.64065620456596406, -28.99954194078535963, 15.00000000000000000 ) ) ;
#6360 = ORIENTED_EDGE ( 'NONE', *, *, #4181, .T. ) ;
#6361 = AXIS2_PLACEMENT_3D ( 'NONE', #2684, #3233, #951 ) ;
#6362 = CIRCLE ( 'NONE', #4825, 46.00000000000000000 ) ;
#6363 = NEXT_ASSEMBLY_USAGE_OCCURRENCE ( 'NAUO1', ' ', ' ', #1928, #2790, $ ) ;
#6364 = NEXT_ASSEMBLY_USAGE_OCCURRENCE ( 'NAUO2', ' ', ' ', #1928, #2008, $ ) ;
#6365 = NEXT_ASSEMBLY_USAGE_OCCURRENCE ( 'NAUO3', ' ', ' ', #1928, #1725, $ ) ;
#6366 = NEXT_ASSEMBLY_USAGE_OCCURRENCE ( 'NAUO4', ' ', ' ', #1928, #1341, $ ) ;
#6367 = NEXT_ASSEMBLY_USAGE_OCCURRENCE ( 'NAUO5', ' ', ' ', #1928, #1341, $ ) ;
#6368 = NEXT_ASSEMBLY_USAGE_OCCURRENCE ( 'NAUO6', ' ', ' ', #1928, #1341, $ ) ;
#6369 = NEXT_ASSEMBLY_USAGE_OCCURRENCE ( 'NAUO7', ' ', ' ', #1928, #1341, $ ) ;
#6370 = NEXT_ASSEMBLY_USAGE_OCCURRENCE ( 'NAUO8', ' ', ' ', #1928, #2864, $ ) ;
#6371 = NEXT_ASSEMBLY_USAGE_OCCURRENCE ( 'NAUO9', ' ', ' ', #1928, #2864, $ ) ;
#6372 = NEXT_ASSEMBLY_USAGE_OCCURRENCE ( 'NAUO10', ' ', ' ', #1928, #2864, $ ) ;
#6373 = NEXT_ASSEMBLY_USAGE_OCCURRENCE ( 'NAUO11', ' ', ' ', #1928, #2864, $ ) ;
#6374 = NEXT_ASSEMBLY_USAGE_OCCURRENCE ( 'NAUO12', ' ', ' ', #1928, #3336, $ ) ;
#6375 = NEXT_ASSEMBLY_USAGE_OCCURRENCE ( 'NAUO13', ' ', ' ', #1928, #3336, $ ) ;
#6376 = NEXT_ASSEMBLY_USAGE_OCCURRENCE ( 'NAUO14', ' ', ' ', #1928, #3336, $ ) ;
#6377 = NEXT_ASSEMBLY_USAGE_OCCURRENCE ( 'NAUO15', ' ', ' ', #1928, #3336, $ ) ;
#6378=COLOUR_RGB('Dark Blue',0.08,0.2,0.34);
#6379=FILL_AREA_STYLE_COLOUR('',#6378);
#6380=FILL_AREA_STYLE('',(#6379));
#6381=SURFACE_STYLE_FILL_AREA(#6380);
#6382=SURFACE_SIDE_STYLE('',(#6381));
#6383=SURFACE_STYLE_USAGE(.BOTH.,#6382);
#6384=PRESENTATION_STYLE_ASSIGNMENT((#6383));
#6385=COLOUR_RGB('Light Blue',0.38,0.62,0.78);
#6386=FILL_AREA_STYLE_COLOUR('',#6385);
#6387=FILL_AREA_STYLE('',(#6386));
#6388=SURFACE_STYLE_FILL_AREA(#6387);
#6389=SURFACE_SIDE_STYLE('',(#6388));
#6390=SURFACE_STYLE_USAGE(.BOTH.,#6389);
#6391=PRESENTATION_STYLE_ASSIGNMENT((#6390));
#6392=COLOUR_RGB('Sky Blue',0.24,0.69,0.87);
#6393=FILL_AREA_STYLE_COLOUR('',#6392);
#6394=FILL_AREA_STYLE('',(#6393));
#6395=SURFACE_STYLE_FILL_AREA(#6394);
#6396=SURFACE_SIDE_STYLE('',(#6395));
#6397=SURFACE_STYLE_USAGE(.BOTH.,#6396);
#6398=PRESENTATION_STYLE_ASSIGNMENT((#6397));
#6399=COLOUR_RGB('Grey',0.48,0.52,0.57);
#6400=FILL_AREA_STYLE_COLOUR('',#6399);
#6401=FILL_AREA_STYLE('',(#6400));
#6402=SURFACE_STYLE_FILL_AREA(#6401);
#6403=SURFACE_SIDE_STYLE('',(#6402));
#6404=SURFACE_STYLE_USAGE(.BOTH.,#6403);
#6405=PRESENTATION_STYLE_ASSIGNMENT((#6404));
#6406=COLOUR_RGB('Black',0.12,0.14,0.17);
#6407=FILL_AREA_STYLE_COLOUR('',#6406);
#6408=FILL_AREA_STYLE('',(#6407));
#6409=SURFACE_STYLE_FILL_AREA(#6408);
#6410=SURFACE_SIDE_STYLE('',(#6409));
#6411=SURFACE_STYLE_USAGE(.BOTH.,#6410);
#6412=PRESENTATION_STYLE_ASSIGNMENT((#6411));
#6413=COLOUR_RGB('Off White',0.89,0.88,0.83);
#6414=FILL_AREA_STYLE_COLOUR('',#6413);
#6415=FILL_AREA_STYLE('',(#6414));
#6416=SURFACE_STYLE_FILL_AREA(#6415);
#6417=SURFACE_SIDE_STYLE('',(#6416));
#6418=SURFACE_STYLE_USAGE(.BOTH.,#6417);
#6419=PRESENTATION_STYLE_ASSIGNMENT((#6418));
ENDSEC;
END-ISO-10303-21;
